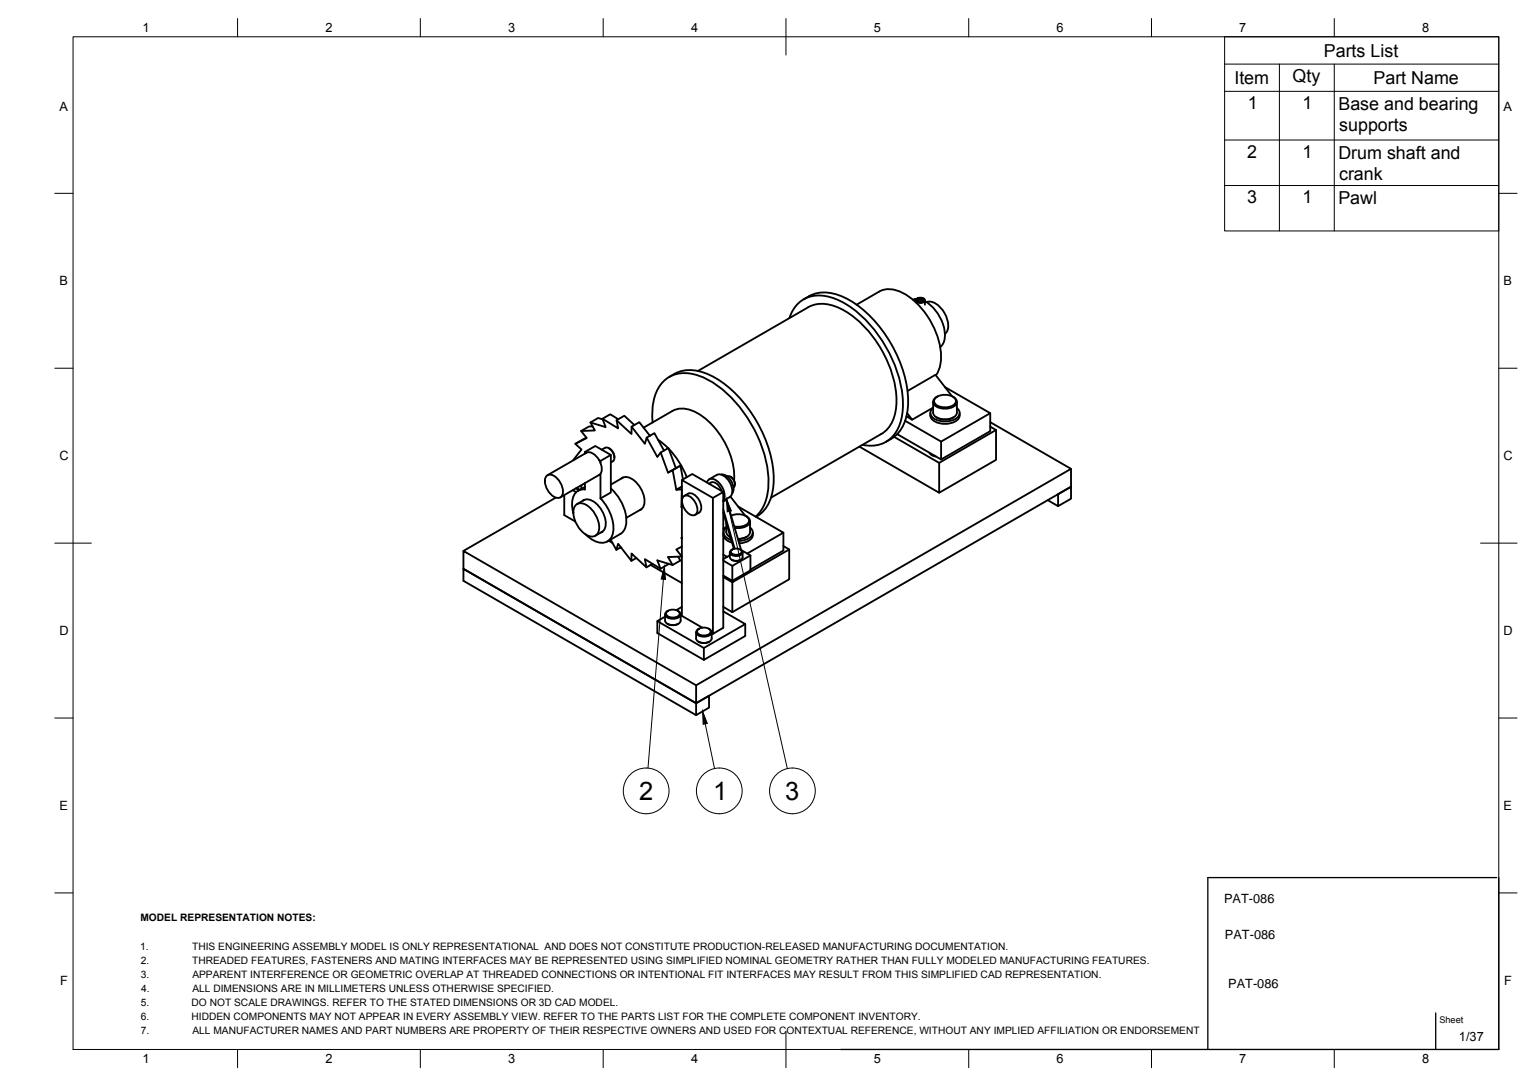
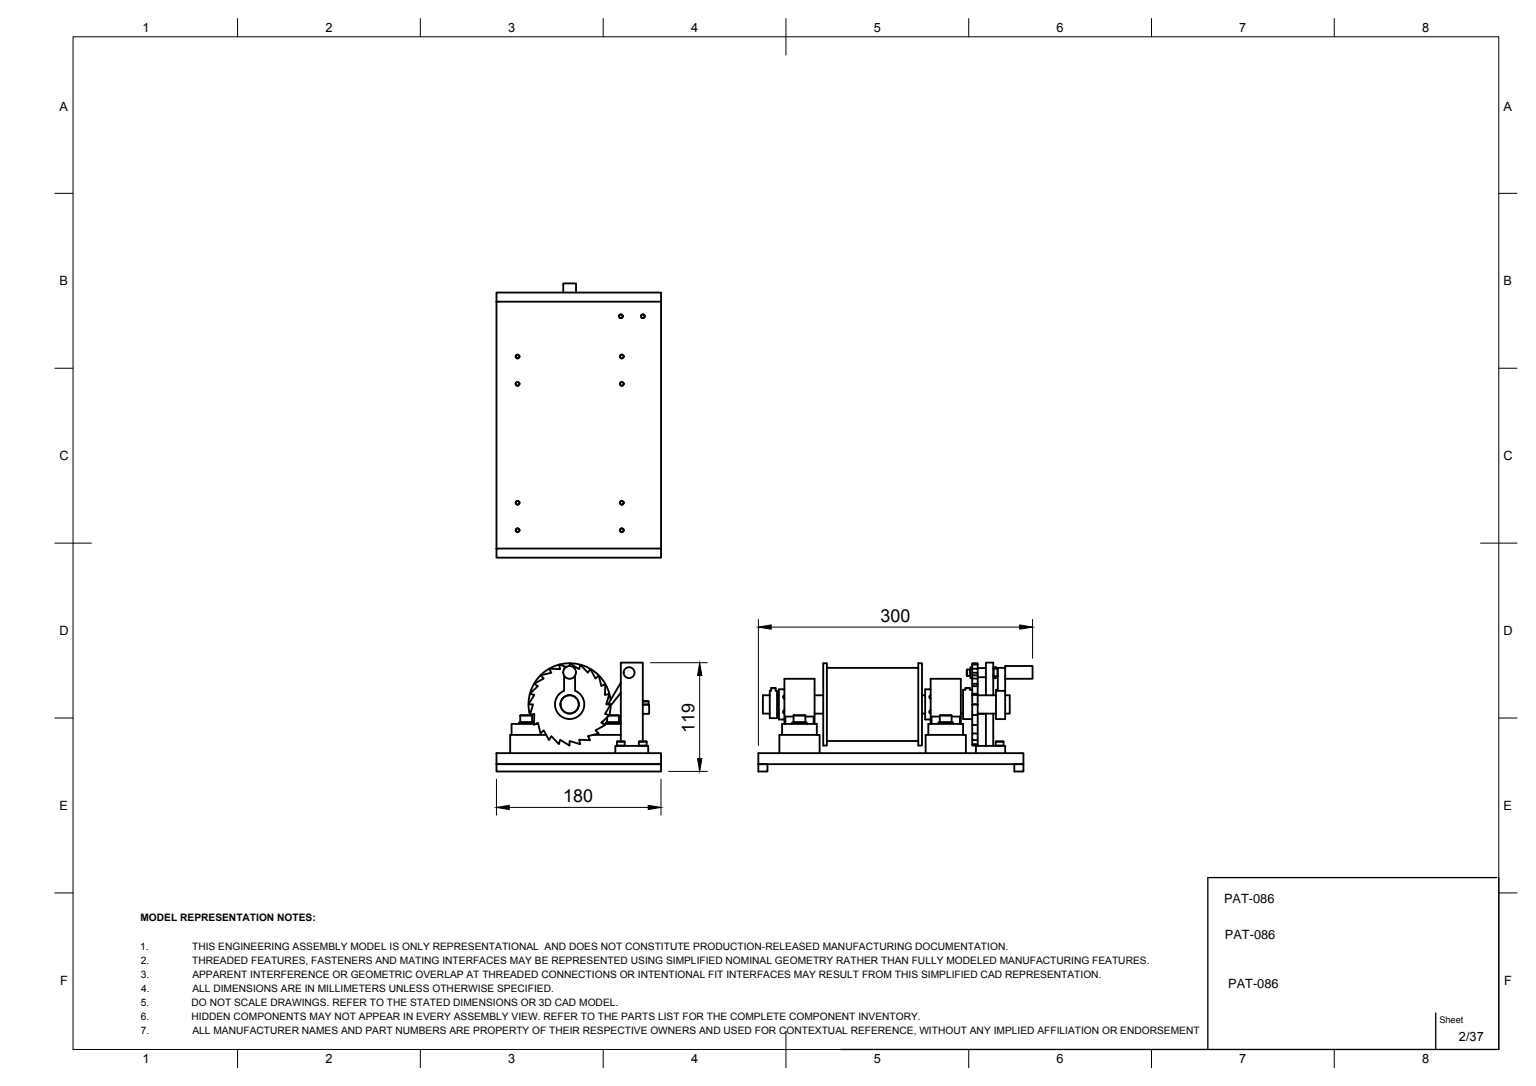
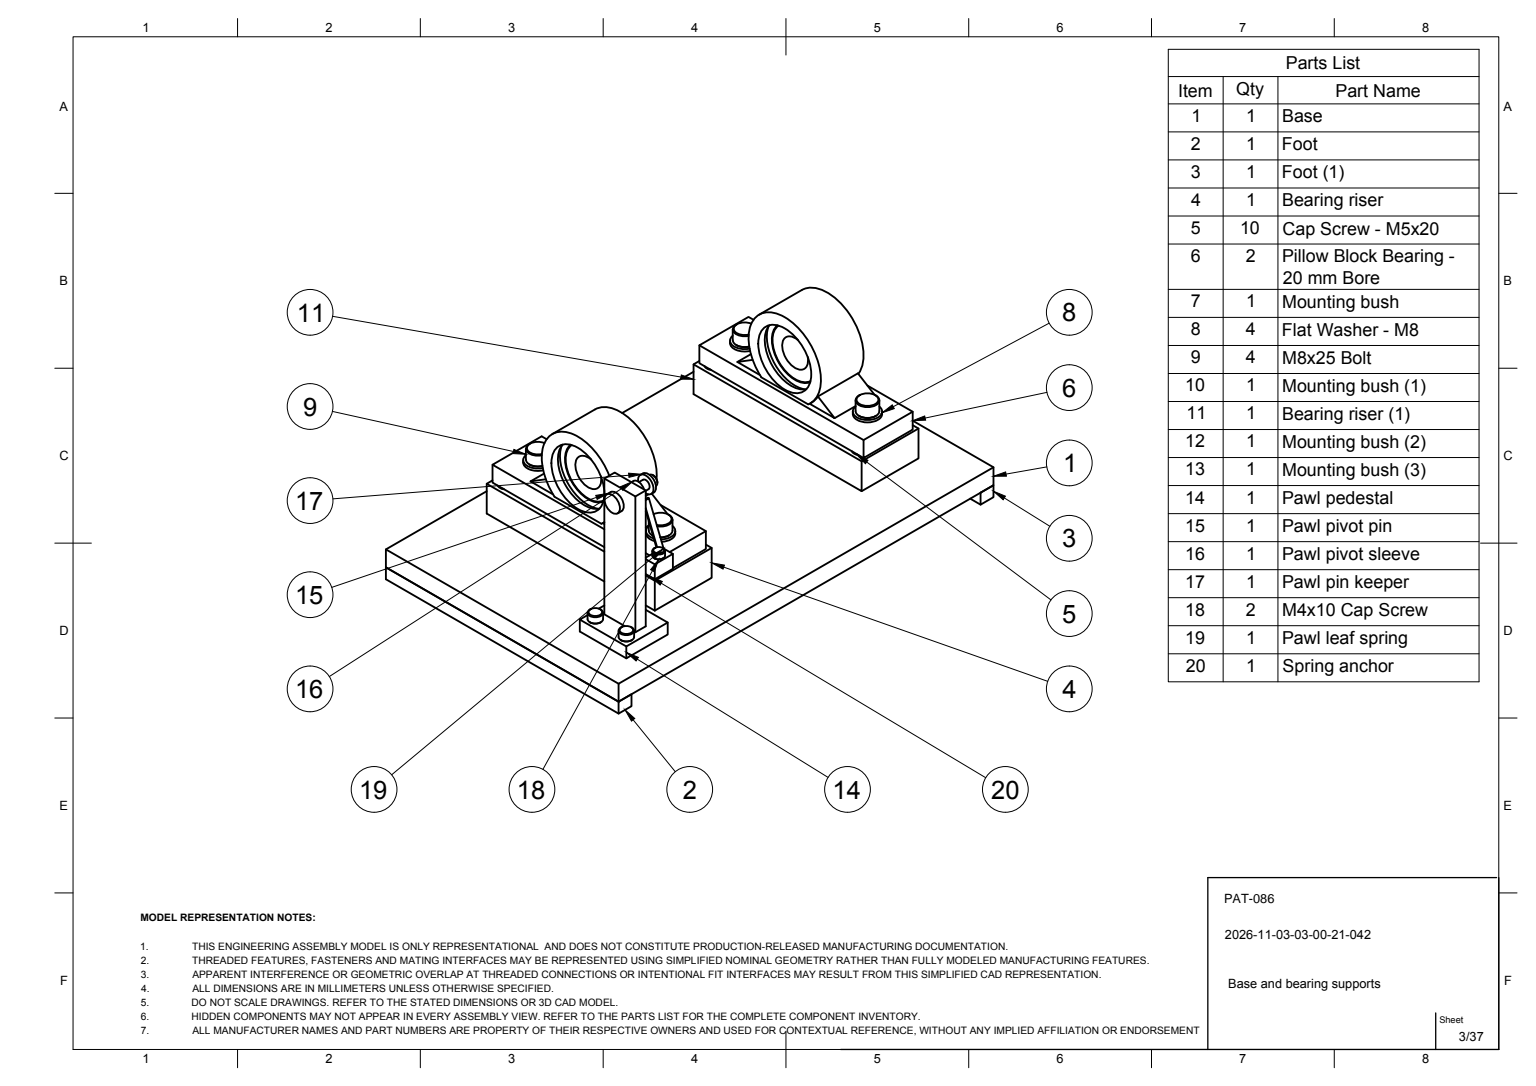
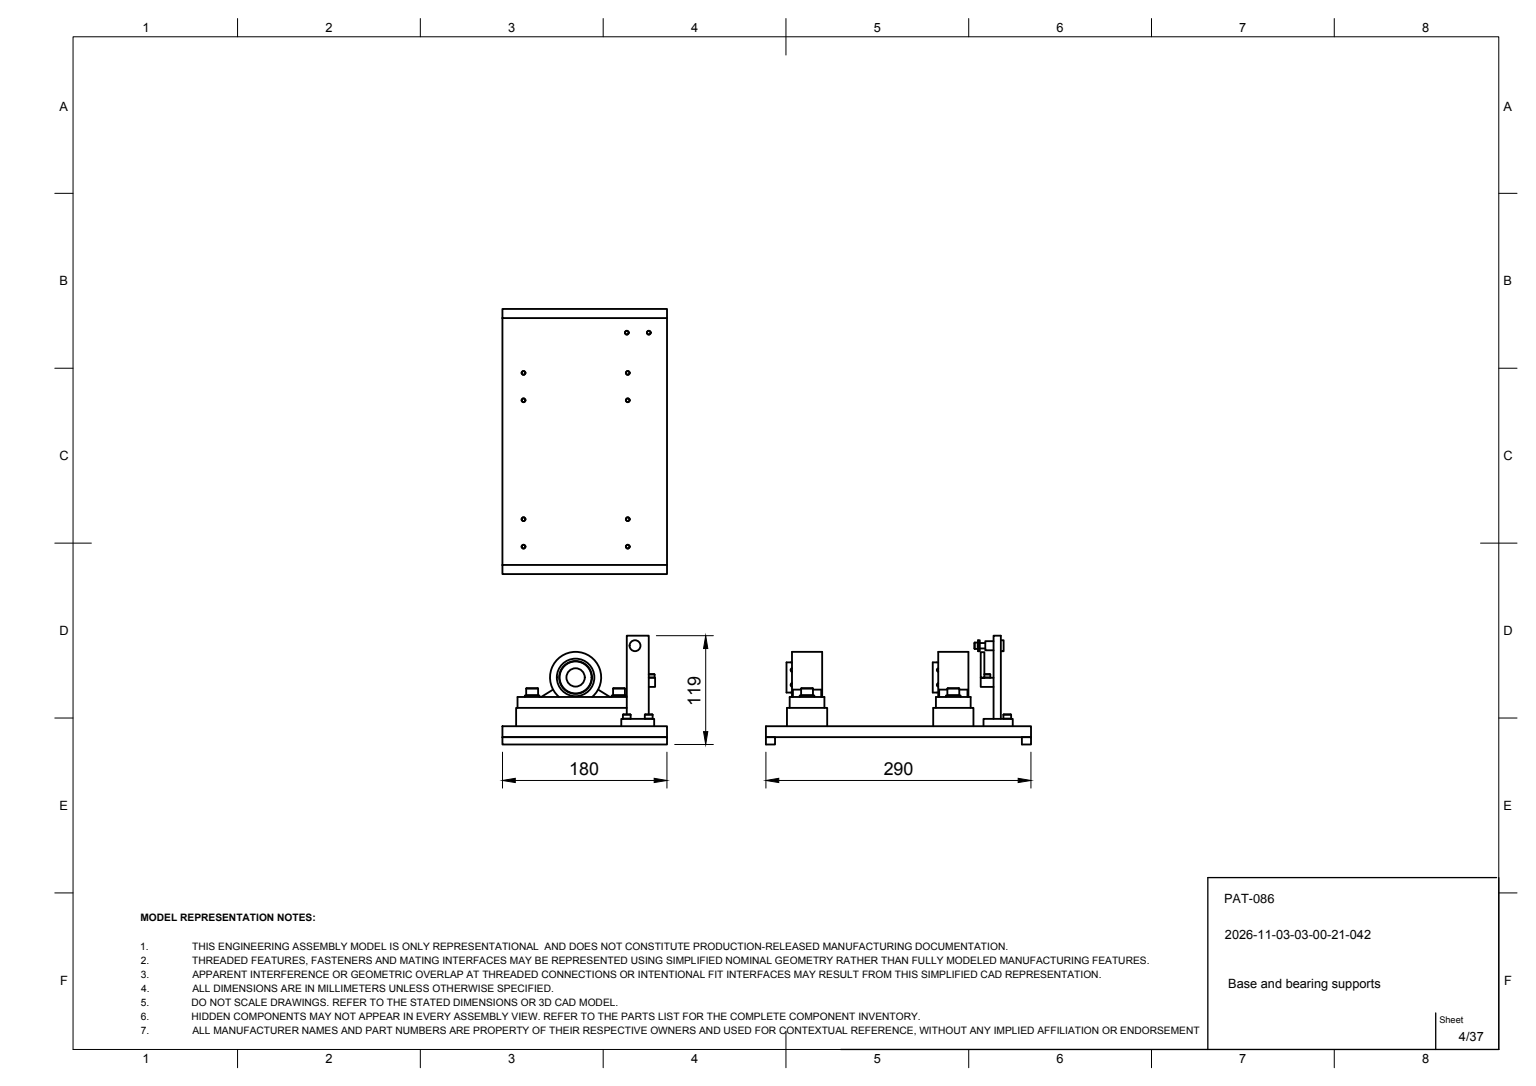
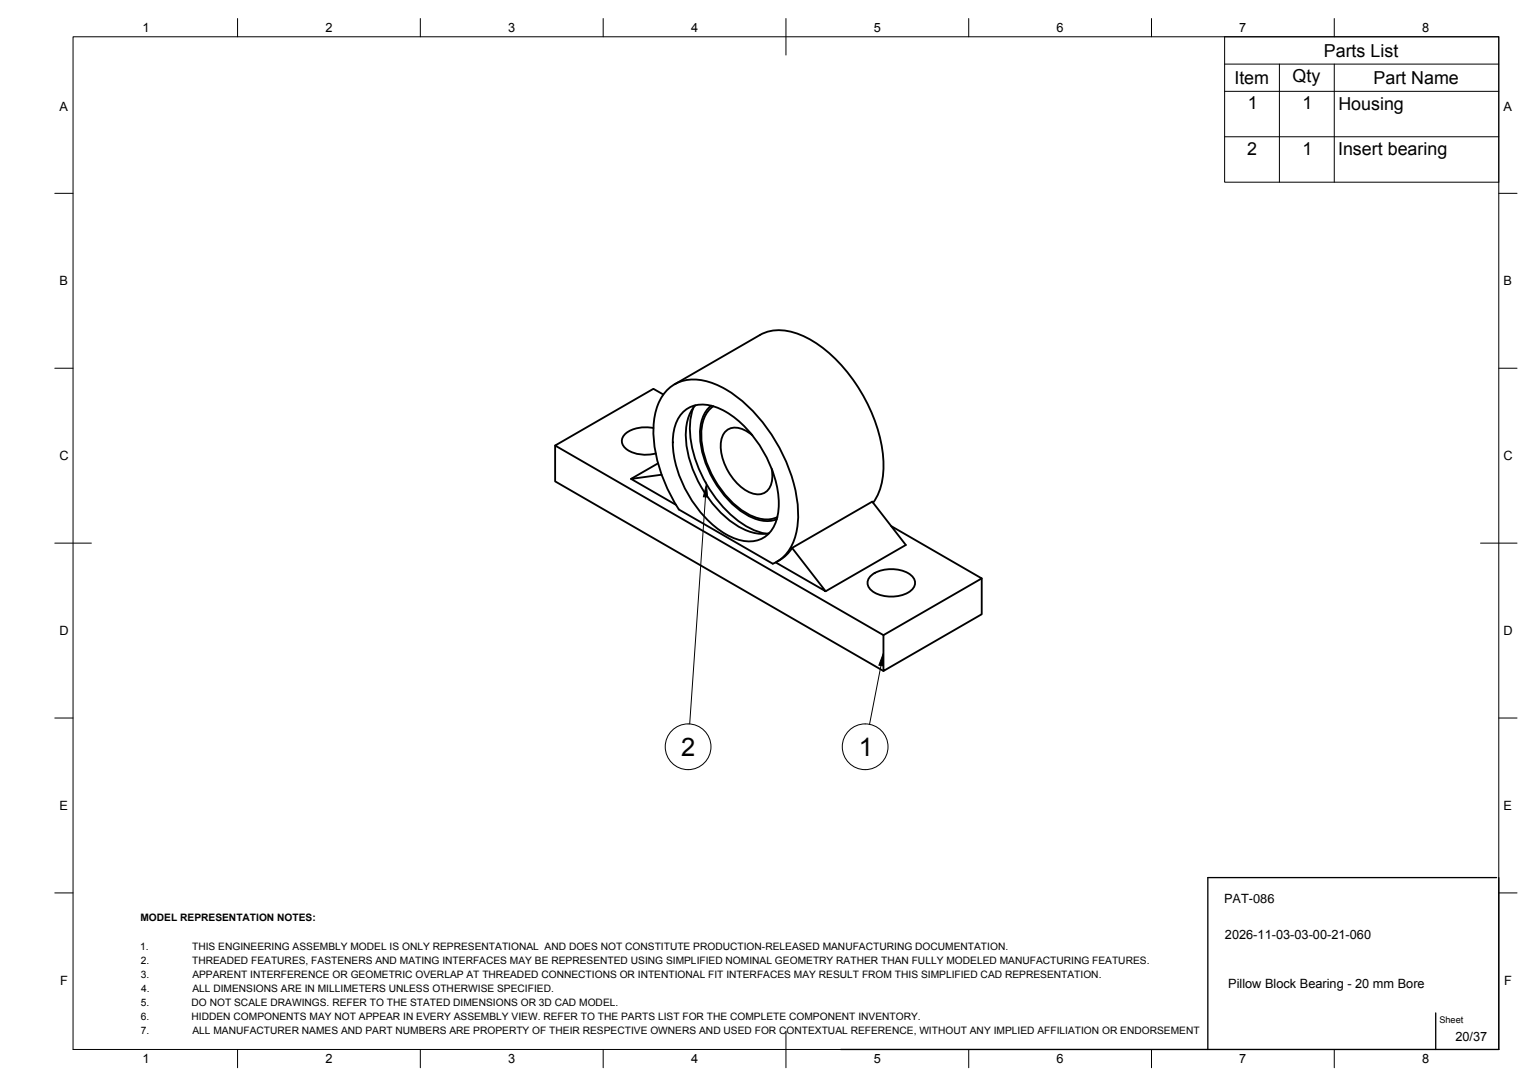
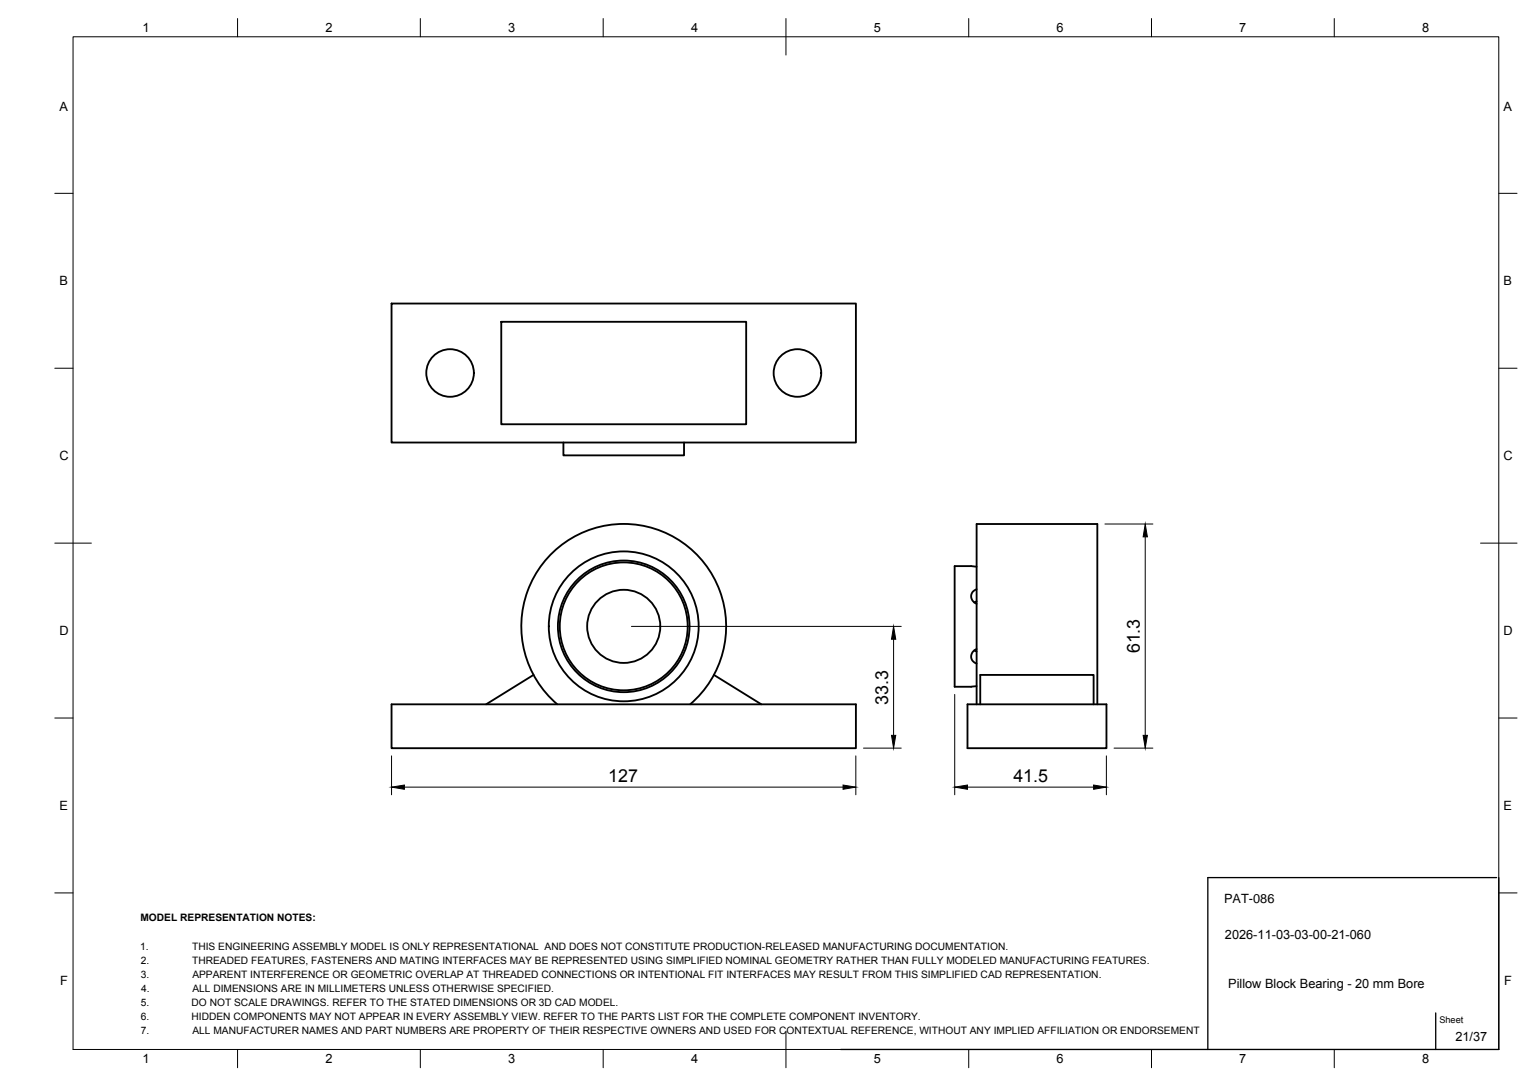
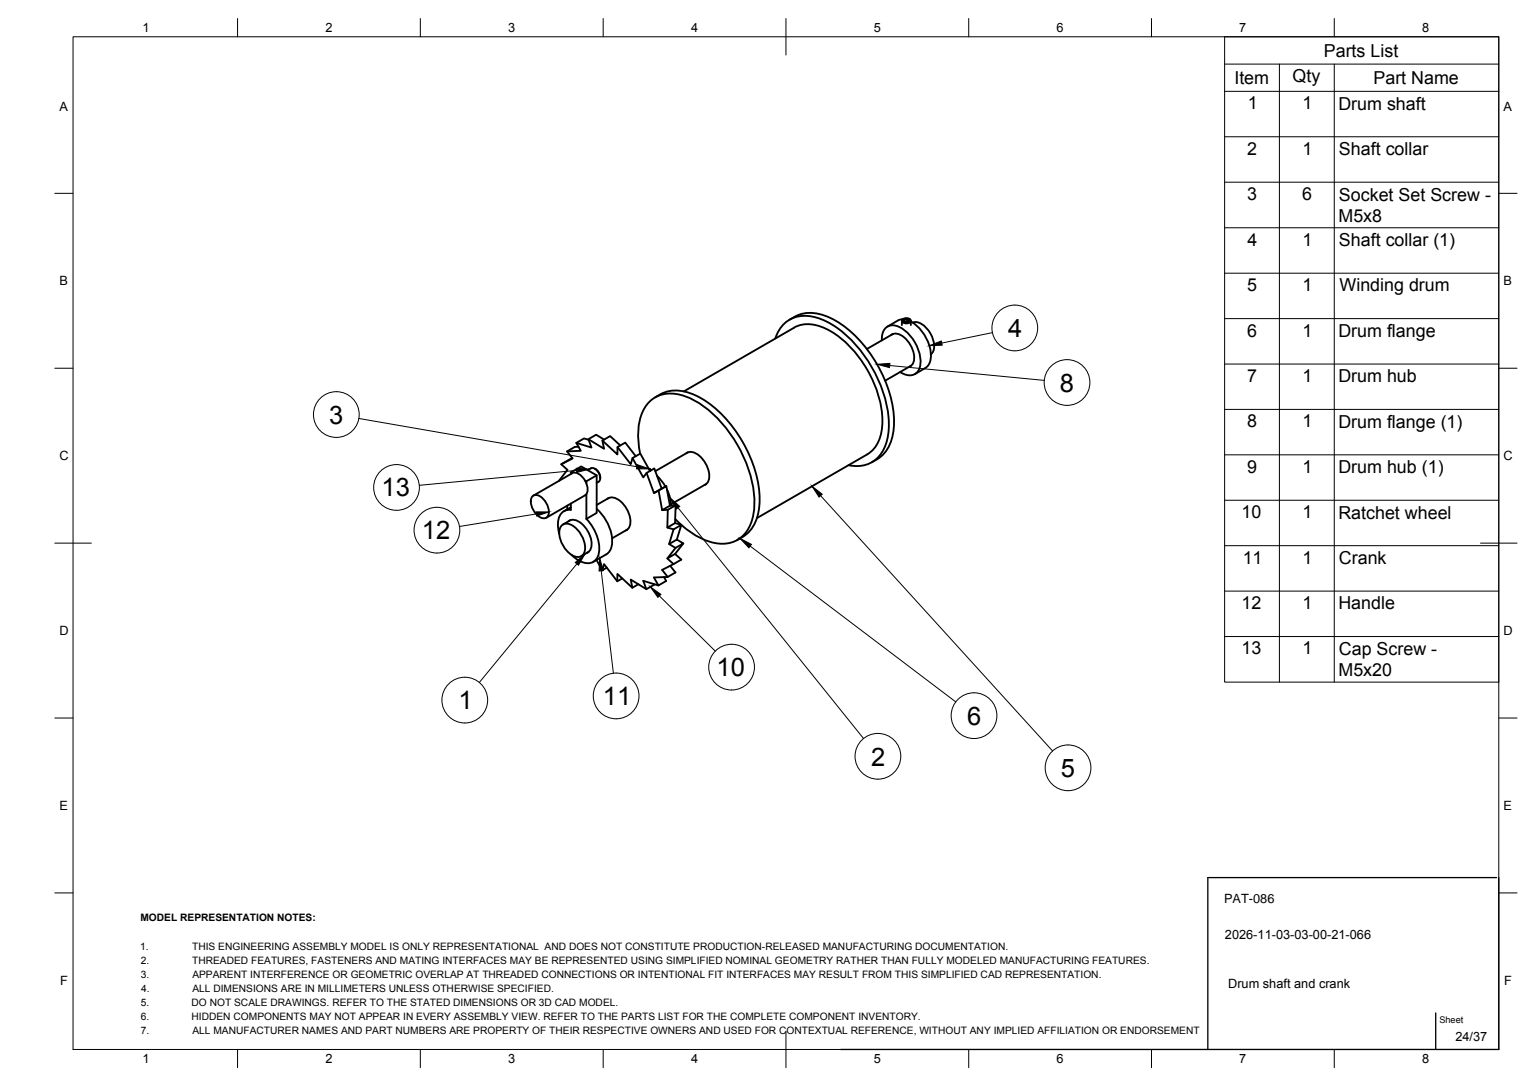
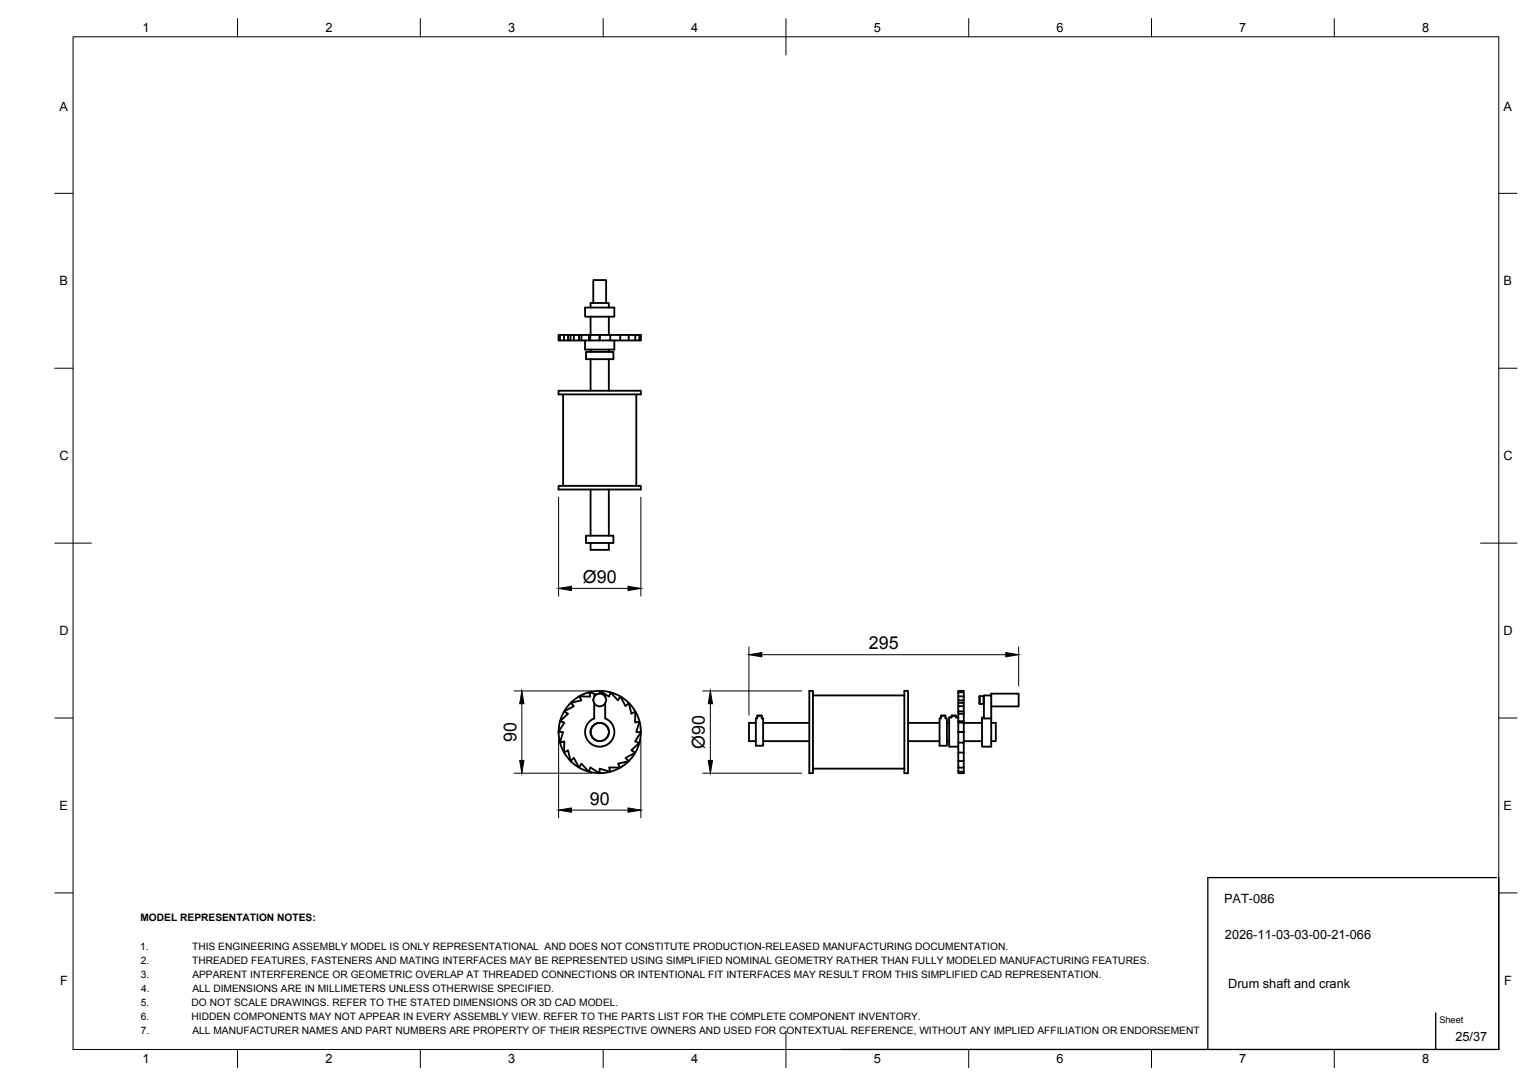
ISO-10303-21;
HEADER;
/* Generated by software containing ST-Developer
 * from STEP Tools, Inc. (www.steptools.com) 
 */

FILE_DESCRIPTION(
/* description */ ('Ratchet and pawl hand winch drum'),
/* implementation_level */ '2;1');

FILE_NAME(
/* name */ 'PAT-086',
/* time_stamp */ '2026-10-27T12:42:58-07:00',
/* author */ (''),
/* organization */ (''),
/* preprocessor_version */ 'ST-DEVELOPER v20.2',
/* originating_system */ 'Autodesk Translation Framework v15.17.0.0',
/* authorisation */ '');

FILE_SCHEMA (('AUTOMOTIVE_DESIGN { 1 0 10303 214 3 1 1 }'));
ENDSEC;

DATA;
#10=MECHANICAL_DESIGN_GEOMETRIC_PRESENTATION_REPRESENTATION('',(#389,#390,
#391,#392,#393,#394,#395,#396,#397,#398,#399,#400,#401,#402,#403,#404,#405,
#406,#407,#408,#409,#410,#411,#412,#413,#414,#415,#416,#417,#418,#419,#420,
#421,#422,#423),#11801);
#11=CONICAL_SURFACE('',#7014,0.625,0.785398163397448);
#12=CONICAL_SURFACE('',#7018,0.635,0.785398163397449);
#13=CONICAL_SURFACE('',#7022,0.41,0.463647609000806);
#14=CONICAL_SURFACE('',#7038,0.325,0.785398163397448);
#15=CONICAL_SURFACE('',#7042,0.335,0.785398163397448);
#16=CONICAL_SURFACE('',#7046,0.21,0.463647609000806);
#17=CONICAL_SURFACE('',#7253,0.235,0.785398163397448);
#18=CONICAL_SURFACE('',#7257,0.2125,0.785398163397448);
#19=CONICAL_SURFACE('',#7263,0.4,0.785398163397448);
#20=CONICAL_SURFACE('',#7267,0.41,0.785398163397448);
#21=CONICAL_SURFACE('',#7271,0.26,0.463647609000806);
#22=CONICAL_SURFACE('',#7275,0.225,0.785398163397448);
#23=ORIENTED_CLOSED_SHELL('',*,#6285,.F.);
#24=ORIENTED_CLOSED_SHELL('',*,#6287,.F.);
#25=ORIENTED_CLOSED_SHELL('',*,#6302,.F.);
#26=BREP_WITH_VOIDS('Body1',#6286,(#23));
#27=BREP_WITH_VOIDS('Body1',#6288,(#24));
#28=BREP_WITH_VOIDS('Body1',#6301,(#25));
#29=ITEM_DEFINED_TRANSFORMATION($,$,#6921,#6990);
#30=ITEM_DEFINED_TRANSFORMATION($,$,#6962,#6991);
#31=ITEM_DEFINED_TRANSFORMATION($,$,#6681,#7286);
#32=ITEM_DEFINED_TRANSFORMATION($,$,#6718,#7287);
#33=ITEM_DEFINED_TRANSFORMATION($,$,#6725,#7288);
#34=ITEM_DEFINED_TRANSFORMATION($,$,#6732,#7289);
#35=ITEM_DEFINED_TRANSFORMATION($,$,#6773,#7290);
#36=ITEM_DEFINED_TRANSFORMATION($,$,#6782,#7291);
#37=ITEM_DEFINED_TRANSFORMATION($,$,#6791,#7292);
#38=ITEM_DEFINED_TRANSFORMATION($,$,#6832,#7293);
#39=ITEM_DEFINED_TRANSFORMATION($,$,#6841,#7294);
#40=ITEM_DEFINED_TRANSFORMATION($,$,#6850,#7295);
#41=ITEM_DEFINED_TRANSFORMATION($,$,#6871,#7296);
#42=ITEM_DEFINED_TRANSFORMATION($,$,#6885,#7297);
#43=ITEM_DEFINED_TRANSFORMATION($,$,#6894,#7298);
#44=ITEM_DEFINED_TRANSFORMATION($,$,#6903,#7299);
#45=ITEM_DEFINED_TRANSFORMATION($,$,#6910,#7300);
#46=ITEM_DEFINED_TRANSFORMATION($,$,#7260,#7301);
#47=ITEM_DEFINED_TRANSFORMATION($,$,#7260,#7302);
#48=ITEM_DEFINED_TRANSFORMATION($,$,#7260,#7303);
#49=ITEM_DEFINED_TRANSFORMATION($,$,#7260,#7304);
#50=ITEM_DEFINED_TRANSFORMATION($,$,#6920,#7305);
#51=ITEM_DEFINED_TRANSFORMATION($,$,#6992,#7306);
#52=ITEM_DEFINED_TRANSFORMATION($,$,#7001,#7307);
#53=ITEM_DEFINED_TRANSFORMATION($,$,#6992,#7308);
#54=ITEM_DEFINED_TRANSFORMATION($,$,#7001,#7309);
#55=ITEM_DEFINED_TRANSFORMATION($,$,#7260,#7310);
#56=ITEM_DEFINED_TRANSFORMATION($,$,#7260,#7311);
#57=ITEM_DEFINED_TRANSFORMATION($,$,#7260,#7312);
#58=ITEM_DEFINED_TRANSFORMATION($,$,#7260,#7313);
#59=ITEM_DEFINED_TRANSFORMATION($,$,#6920,#7314);
#60=ITEM_DEFINED_TRANSFORMATION($,$,#6992,#7315);
#61=ITEM_DEFINED_TRANSFORMATION($,$,#7001,#7316);
#62=ITEM_DEFINED_TRANSFORMATION($,$,#6992,#7317);
#63=ITEM_DEFINED_TRANSFORMATION($,$,#7001,#7318);
#64=ITEM_DEFINED_TRANSFORMATION($,$,#7260,#7319);
#65=ITEM_DEFINED_TRANSFORMATION($,$,#7260,#7320);
#66=ITEM_DEFINED_TRANSFORMATION($,$,#7025,#7321);
#67=ITEM_DEFINED_TRANSFORMATION($,$,#7025,#7322);
#68=ITEM_DEFINED_TRANSFORMATION($,$,#7050,#7323);
#69=ITEM_DEFINED_TRANSFORMATION($,$,#7056,#7324);
#70=ITEM_DEFINED_TRANSFORMATION($,$,#7071,#7325);
#71=ITEM_DEFINED_TRANSFORMATION($,$,#7086,#7326);
#72=ITEM_DEFINED_TRANSFORMATION($,$,#7095,#7327);
#73=ITEM_DEFINED_TRANSFORMATION($,$,#7104,#7328);
#74=ITEM_DEFINED_TRANSFORMATION($,$,#7119,#7329);
#75=ITEM_DEFINED_TRANSFORMATION($,$,#7128,#7330);
#76=ITEM_DEFINED_TRANSFORMATION($,$,#7143,#7331);
#77=ITEM_DEFINED_TRANSFORMATION($,$,#7207,#7332);
#78=ITEM_DEFINED_TRANSFORMATION($,$,#7233,#7333);
#79=ITEM_DEFINED_TRANSFORMATION($,$,#7243,#7334);
#80=ITEM_DEFINED_TRANSFORMATION($,$,#7243,#7335);
#81=ITEM_DEFINED_TRANSFORMATION($,$,#7243,#7336);
#82=ITEM_DEFINED_TRANSFORMATION($,$,#7243,#7337);
#83=ITEM_DEFINED_TRANSFORMATION($,$,#7243,#7338);
#84=ITEM_DEFINED_TRANSFORMATION($,$,#7243,#7339);
#85=ITEM_DEFINED_TRANSFORMATION($,$,#7260,#7340);
#86=ITEM_DEFINED_TRANSFORMATION($,$,#7342,#7354);
#87=ITEM_DEFINED_TRANSFORMATION($,$,#6680,#7355);
#88=ITEM_DEFINED_TRANSFORMATION($,$,#7049,#7356);
#89=ITEM_DEFINED_TRANSFORMATION($,$,#7341,#7357);
#90=(
REPRESENTATION_RELATIONSHIP($,$,#11963,#11962)
REPRESENTATION_RELATIONSHIP_WITH_TRANSFORMATION(#29)
SHAPE_REPRESENTATION_RELATIONSHIP()
);
#91=(
REPRESENTATION_RELATIONSHIP($,$,#11964,#11962)
REPRESENTATION_RELATIONSHIP_WITH_TRANSFORMATION(#30)
SHAPE_REPRESENTATION_RELATIONSHIP()
);
#92=(
REPRESENTATION_RELATIONSHIP($,$,#11947,#11946)
REPRESENTATION_RELATIONSHIP_WITH_TRANSFORMATION(#31)
SHAPE_REPRESENTATION_RELATIONSHIP()
);
#93=(
REPRESENTATION_RELATIONSHIP($,$,#11948,#11946)
REPRESENTATION_RELATIONSHIP_WITH_TRANSFORMATION(#32)
SHAPE_REPRESENTATION_RELATIONSHIP()
);
#94=(
REPRESENTATION_RELATIONSHIP($,$,#11949,#11946)
REPRESENTATION_RELATIONSHIP_WITH_TRANSFORMATION(#33)
SHAPE_REPRESENTATION_RELATIONSHIP()
);
#95=(
REPRESENTATION_RELATIONSHIP($,$,#11950,#11946)
REPRESENTATION_RELATIONSHIP_WITH_TRANSFORMATION(#34)
SHAPE_REPRESENTATION_RELATIONSHIP()
);
#96=(
REPRESENTATION_RELATIONSHIP($,$,#11951,#11946)
REPRESENTATION_RELATIONSHIP_WITH_TRANSFORMATION(#35)
SHAPE_REPRESENTATION_RELATIONSHIP()
);
#97=(
REPRESENTATION_RELATIONSHIP($,$,#11952,#11946)
REPRESENTATION_RELATIONSHIP_WITH_TRANSFORMATION(#36)
SHAPE_REPRESENTATION_RELATIONSHIP()
);
#98=(
REPRESENTATION_RELATIONSHIP($,$,#11953,#11946)
REPRESENTATION_RELATIONSHIP_WITH_TRANSFORMATION(#37)
SHAPE_REPRESENTATION_RELATIONSHIP()
);
#99=(
REPRESENTATION_RELATIONSHIP($,$,#11954,#11946)
REPRESENTATION_RELATIONSHIP_WITH_TRANSFORMATION(#38)
SHAPE_REPRESENTATION_RELATIONSHIP()
);
#100=(
REPRESENTATION_RELATIONSHIP($,$,#11955,#11946)
REPRESENTATION_RELATIONSHIP_WITH_TRANSFORMATION(#39)
SHAPE_REPRESENTATION_RELATIONSHIP()
);
#101=(
REPRESENTATION_RELATIONSHIP($,$,#11956,#11946)
REPRESENTATION_RELATIONSHIP_WITH_TRANSFORMATION(#40)
SHAPE_REPRESENTATION_RELATIONSHIP()
);
#102=(
REPRESENTATION_RELATIONSHIP($,$,#11957,#11946)
REPRESENTATION_RELATIONSHIP_WITH_TRANSFORMATION(#41)
SHAPE_REPRESENTATION_RELATIONSHIP()
);
#103=(
REPRESENTATION_RELATIONSHIP($,$,#11958,#11946)
REPRESENTATION_RELATIONSHIP_WITH_TRANSFORMATION(#42)
SHAPE_REPRESENTATION_RELATIONSHIP()
);
#104=(
REPRESENTATION_RELATIONSHIP($,$,#11959,#11946)
REPRESENTATION_RELATIONSHIP_WITH_TRANSFORMATION(#43)
SHAPE_REPRESENTATION_RELATIONSHIP()
);
#105=(
REPRESENTATION_RELATIONSHIP($,$,#11960,#11946)
REPRESENTATION_RELATIONSHIP_WITH_TRANSFORMATION(#44)
SHAPE_REPRESENTATION_RELATIONSHIP()
);
#106=(
REPRESENTATION_RELATIONSHIP($,$,#11961,#11946)
REPRESENTATION_RELATIONSHIP_WITH_TRANSFORMATION(#45)
SHAPE_REPRESENTATION_RELATIONSHIP()
);
#107=(
REPRESENTATION_RELATIONSHIP($,$,#11981,#11946)
REPRESENTATION_RELATIONSHIP_WITH_TRANSFORMATION(#46)
SHAPE_REPRESENTATION_RELATIONSHIP()
);
#108=(
REPRESENTATION_RELATIONSHIP($,$,#11981,#11946)
REPRESENTATION_RELATIONSHIP_WITH_TRANSFORMATION(#47)
SHAPE_REPRESENTATION_RELATIONSHIP()
);
#109=(
REPRESENTATION_RELATIONSHIP($,$,#11981,#11946)
REPRESENTATION_RELATIONSHIP_WITH_TRANSFORMATION(#48)
SHAPE_REPRESENTATION_RELATIONSHIP()
);
#110=(
REPRESENTATION_RELATIONSHIP($,$,#11981,#11946)
REPRESENTATION_RELATIONSHIP_WITH_TRANSFORMATION(#49)
SHAPE_REPRESENTATION_RELATIONSHIP()
);
#111=(
REPRESENTATION_RELATIONSHIP($,$,#11962,#11946)
REPRESENTATION_RELATIONSHIP_WITH_TRANSFORMATION(#50)
SHAPE_REPRESENTATION_RELATIONSHIP()
);
#112=(
REPRESENTATION_RELATIONSHIP($,$,#11965,#11946)
REPRESENTATION_RELATIONSHIP_WITH_TRANSFORMATION(#51)
SHAPE_REPRESENTATION_RELATIONSHIP()
);
#113=(
REPRESENTATION_RELATIONSHIP($,$,#11966,#11946)
REPRESENTATION_RELATIONSHIP_WITH_TRANSFORMATION(#52)
SHAPE_REPRESENTATION_RELATIONSHIP()
);
#114=(
REPRESENTATION_RELATIONSHIP($,$,#11965,#11946)
REPRESENTATION_RELATIONSHIP_WITH_TRANSFORMATION(#53)
SHAPE_REPRESENTATION_RELATIONSHIP()
);
#115=(
REPRESENTATION_RELATIONSHIP($,$,#11966,#11946)
REPRESENTATION_RELATIONSHIP_WITH_TRANSFORMATION(#54)
SHAPE_REPRESENTATION_RELATIONSHIP()
);
#116=(
REPRESENTATION_RELATIONSHIP($,$,#11981,#11946)
REPRESENTATION_RELATIONSHIP_WITH_TRANSFORMATION(#55)
SHAPE_REPRESENTATION_RELATIONSHIP()
);
#117=(
REPRESENTATION_RELATIONSHIP($,$,#11981,#11946)
REPRESENTATION_RELATIONSHIP_WITH_TRANSFORMATION(#56)
SHAPE_REPRESENTATION_RELATIONSHIP()
);
#118=(
REPRESENTATION_RELATIONSHIP($,$,#11981,#11946)
REPRESENTATION_RELATIONSHIP_WITH_TRANSFORMATION(#57)
SHAPE_REPRESENTATION_RELATIONSHIP()
);
#119=(
REPRESENTATION_RELATIONSHIP($,$,#11981,#11946)
REPRESENTATION_RELATIONSHIP_WITH_TRANSFORMATION(#58)
SHAPE_REPRESENTATION_RELATIONSHIP()
);
#120=(
REPRESENTATION_RELATIONSHIP($,$,#11962,#11946)
REPRESENTATION_RELATIONSHIP_WITH_TRANSFORMATION(#59)
SHAPE_REPRESENTATION_RELATIONSHIP()
);
#121=(
REPRESENTATION_RELATIONSHIP($,$,#11965,#11946)
REPRESENTATION_RELATIONSHIP_WITH_TRANSFORMATION(#60)
SHAPE_REPRESENTATION_RELATIONSHIP()
);
#122=(
REPRESENTATION_RELATIONSHIP($,$,#11966,#11946)
REPRESENTATION_RELATIONSHIP_WITH_TRANSFORMATION(#61)
SHAPE_REPRESENTATION_RELATIONSHIP()
);
#123=(
REPRESENTATION_RELATIONSHIP($,$,#11965,#11946)
REPRESENTATION_RELATIONSHIP_WITH_TRANSFORMATION(#62)
SHAPE_REPRESENTATION_RELATIONSHIP()
);
#124=(
REPRESENTATION_RELATIONSHIP($,$,#11966,#11946)
REPRESENTATION_RELATIONSHIP_WITH_TRANSFORMATION(#63)
SHAPE_REPRESENTATION_RELATIONSHIP()
);
#125=(
REPRESENTATION_RELATIONSHIP($,$,#11981,#11946)
REPRESENTATION_RELATIONSHIP_WITH_TRANSFORMATION(#64)
SHAPE_REPRESENTATION_RELATIONSHIP()
);
#126=(
REPRESENTATION_RELATIONSHIP($,$,#11981,#11946)
REPRESENTATION_RELATIONSHIP_WITH_TRANSFORMATION(#65)
SHAPE_REPRESENTATION_RELATIONSHIP()
);
#127=(
REPRESENTATION_RELATIONSHIP($,$,#11967,#11946)
REPRESENTATION_RELATIONSHIP_WITH_TRANSFORMATION(#66)
SHAPE_REPRESENTATION_RELATIONSHIP()
);
#128=(
REPRESENTATION_RELATIONSHIP($,$,#11967,#11946)
REPRESENTATION_RELATIONSHIP_WITH_TRANSFORMATION(#67)
SHAPE_REPRESENTATION_RELATIONSHIP()
);
#129=(
REPRESENTATION_RELATIONSHIP($,$,#11969,#11968)
REPRESENTATION_RELATIONSHIP_WITH_TRANSFORMATION(#68)
SHAPE_REPRESENTATION_RELATIONSHIP()
);
#130=(
REPRESENTATION_RELATIONSHIP($,$,#11970,#11968)
REPRESENTATION_RELATIONSHIP_WITH_TRANSFORMATION(#69)
SHAPE_REPRESENTATION_RELATIONSHIP()
);
#131=(
REPRESENTATION_RELATIONSHIP($,$,#11971,#11968)
REPRESENTATION_RELATIONSHIP_WITH_TRANSFORMATION(#70)
SHAPE_REPRESENTATION_RELATIONSHIP()
);
#132=(
REPRESENTATION_RELATIONSHIP($,$,#11972,#11968)
REPRESENTATION_RELATIONSHIP_WITH_TRANSFORMATION(#71)
SHAPE_REPRESENTATION_RELATIONSHIP()
);
#133=(
REPRESENTATION_RELATIONSHIP($,$,#11973,#11968)
REPRESENTATION_RELATIONSHIP_WITH_TRANSFORMATION(#72)
SHAPE_REPRESENTATION_RELATIONSHIP()
);
#134=(
REPRESENTATION_RELATIONSHIP($,$,#11974,#11968)
REPRESENTATION_RELATIONSHIP_WITH_TRANSFORMATION(#73)
SHAPE_REPRESENTATION_RELATIONSHIP()
);
#135=(
REPRESENTATION_RELATIONSHIP($,$,#11975,#11968)
REPRESENTATION_RELATIONSHIP_WITH_TRANSFORMATION(#74)
SHAPE_REPRESENTATION_RELATIONSHIP()
);
#136=(
REPRESENTATION_RELATIONSHIP($,$,#11976,#11968)
REPRESENTATION_RELATIONSHIP_WITH_TRANSFORMATION(#75)
SHAPE_REPRESENTATION_RELATIONSHIP()
);
#137=(
REPRESENTATION_RELATIONSHIP($,$,#11977,#11968)
REPRESENTATION_RELATIONSHIP_WITH_TRANSFORMATION(#76)
SHAPE_REPRESENTATION_RELATIONSHIP()
);
#138=(
REPRESENTATION_RELATIONSHIP($,$,#11978,#11968)
REPRESENTATION_RELATIONSHIP_WITH_TRANSFORMATION(#77)
SHAPE_REPRESENTATION_RELATIONSHIP()
);
#139=(
REPRESENTATION_RELATIONSHIP($,$,#11979,#11968)
REPRESENTATION_RELATIONSHIP_WITH_TRANSFORMATION(#78)
SHAPE_REPRESENTATION_RELATIONSHIP()
);
#140=(
REPRESENTATION_RELATIONSHIP($,$,#11980,#11968)
REPRESENTATION_RELATIONSHIP_WITH_TRANSFORMATION(#79)
SHAPE_REPRESENTATION_RELATIONSHIP()
);
#141=(
REPRESENTATION_RELATIONSHIP($,$,#11980,#11968)
REPRESENTATION_RELATIONSHIP_WITH_TRANSFORMATION(#80)
SHAPE_REPRESENTATION_RELATIONSHIP()
);
#142=(
REPRESENTATION_RELATIONSHIP($,$,#11980,#11968)
REPRESENTATION_RELATIONSHIP_WITH_TRANSFORMATION(#81)
SHAPE_REPRESENTATION_RELATIONSHIP()
);
#143=(
REPRESENTATION_RELATIONSHIP($,$,#11980,#11968)
REPRESENTATION_RELATIONSHIP_WITH_TRANSFORMATION(#82)
SHAPE_REPRESENTATION_RELATIONSHIP()
);
#144=(
REPRESENTATION_RELATIONSHIP($,$,#11980,#11968)
REPRESENTATION_RELATIONSHIP_WITH_TRANSFORMATION(#83)
SHAPE_REPRESENTATION_RELATIONSHIP()
);
#145=(
REPRESENTATION_RELATIONSHIP($,$,#11980,#11968)
REPRESENTATION_RELATIONSHIP_WITH_TRANSFORMATION(#84)
SHAPE_REPRESENTATION_RELATIONSHIP()
);
#146=(
REPRESENTATION_RELATIONSHIP($,$,#11981,#11968)
REPRESENTATION_RELATIONSHIP_WITH_TRANSFORMATION(#85)
SHAPE_REPRESENTATION_RELATIONSHIP()
);
#147=(
REPRESENTATION_RELATIONSHIP($,$,#11983,#11982)
REPRESENTATION_RELATIONSHIP_WITH_TRANSFORMATION(#86)
SHAPE_REPRESENTATION_RELATIONSHIP()
);
#148=(
REPRESENTATION_RELATIONSHIP($,$,#11946,#11945)
REPRESENTATION_RELATIONSHIP_WITH_TRANSFORMATION(#87)
SHAPE_REPRESENTATION_RELATIONSHIP()
);
#149=(
REPRESENTATION_RELATIONSHIP($,$,#11968,#11945)
REPRESENTATION_RELATIONSHIP_WITH_TRANSFORMATION(#88)
SHAPE_REPRESENTATION_RELATIONSHIP()
);
#150=(
REPRESENTATION_RELATIONSHIP($,$,#11982,#11945)
REPRESENTATION_RELATIONSHIP_WITH_TRANSFORMATION(#89)
SHAPE_REPRESENTATION_RELATIONSHIP()
);
#151=CONTEXT_DEPENDENT_SHAPE_REPRESENTATION(#90,#11865);
#152=CONTEXT_DEPENDENT_SHAPE_REPRESENTATION(#91,#11866);
#153=CONTEXT_DEPENDENT_SHAPE_REPRESENTATION(#92,#11884);
#154=CONTEXT_DEPENDENT_SHAPE_REPRESENTATION(#93,#11885);
#155=CONTEXT_DEPENDENT_SHAPE_REPRESENTATION(#94,#11886);
#156=CONTEXT_DEPENDENT_SHAPE_REPRESENTATION(#95,#11887);
#157=CONTEXT_DEPENDENT_SHAPE_REPRESENTATION(#96,#11888);
#158=CONTEXT_DEPENDENT_SHAPE_REPRESENTATION(#97,#11889);
#159=CONTEXT_DEPENDENT_SHAPE_REPRESENTATION(#98,#11890);
#160=CONTEXT_DEPENDENT_SHAPE_REPRESENTATION(#99,#11891);
#161=CONTEXT_DEPENDENT_SHAPE_REPRESENTATION(#100,#11892);
#162=CONTEXT_DEPENDENT_SHAPE_REPRESENTATION(#101,#11893);
#163=CONTEXT_DEPENDENT_SHAPE_REPRESENTATION(#102,#11894);
#164=CONTEXT_DEPENDENT_SHAPE_REPRESENTATION(#103,#11895);
#165=CONTEXT_DEPENDENT_SHAPE_REPRESENTATION(#104,#11896);
#166=CONTEXT_DEPENDENT_SHAPE_REPRESENTATION(#105,#11897);
#167=CONTEXT_DEPENDENT_SHAPE_REPRESENTATION(#106,#11898);
#168=CONTEXT_DEPENDENT_SHAPE_REPRESENTATION(#107,#11899);
#169=CONTEXT_DEPENDENT_SHAPE_REPRESENTATION(#108,#11900);
#170=CONTEXT_DEPENDENT_SHAPE_REPRESENTATION(#109,#11901);
#171=CONTEXT_DEPENDENT_SHAPE_REPRESENTATION(#110,#11902);
#172=CONTEXT_DEPENDENT_SHAPE_REPRESENTATION(#111,#11903);
#173=CONTEXT_DEPENDENT_SHAPE_REPRESENTATION(#112,#11904);
#174=CONTEXT_DEPENDENT_SHAPE_REPRESENTATION(#113,#11905);
#175=CONTEXT_DEPENDENT_SHAPE_REPRESENTATION(#114,#11906);
#176=CONTEXT_DEPENDENT_SHAPE_REPRESENTATION(#115,#11907);
#177=CONTEXT_DEPENDENT_SHAPE_REPRESENTATION(#116,#11908);
#178=CONTEXT_DEPENDENT_SHAPE_REPRESENTATION(#117,#11909);
#179=CONTEXT_DEPENDENT_SHAPE_REPRESENTATION(#118,#11910);
#180=CONTEXT_DEPENDENT_SHAPE_REPRESENTATION(#119,#11911);
#181=CONTEXT_DEPENDENT_SHAPE_REPRESENTATION(#120,#11912);
#182=CONTEXT_DEPENDENT_SHAPE_REPRESENTATION(#121,#11913);
#183=CONTEXT_DEPENDENT_SHAPE_REPRESENTATION(#122,#11914);
#184=CONTEXT_DEPENDENT_SHAPE_REPRESENTATION(#123,#11915);
#185=CONTEXT_DEPENDENT_SHAPE_REPRESENTATION(#124,#11916);
#186=CONTEXT_DEPENDENT_SHAPE_REPRESENTATION(#125,#11917);
#187=CONTEXT_DEPENDENT_SHAPE_REPRESENTATION(#126,#11918);
#188=CONTEXT_DEPENDENT_SHAPE_REPRESENTATION(#127,#11919);
#189=CONTEXT_DEPENDENT_SHAPE_REPRESENTATION(#128,#11920);
#190=CONTEXT_DEPENDENT_SHAPE_REPRESENTATION(#129,#11921);
#191=CONTEXT_DEPENDENT_SHAPE_REPRESENTATION(#130,#11922);
#192=CONTEXT_DEPENDENT_SHAPE_REPRESENTATION(#131,#11923);
#193=CONTEXT_DEPENDENT_SHAPE_REPRESENTATION(#132,#11924);
#194=CONTEXT_DEPENDENT_SHAPE_REPRESENTATION(#133,#11925);
#195=CONTEXT_DEPENDENT_SHAPE_REPRESENTATION(#134,#11926);
#196=CONTEXT_DEPENDENT_SHAPE_REPRESENTATION(#135,#11927);
#197=CONTEXT_DEPENDENT_SHAPE_REPRESENTATION(#136,#11928);
#198=CONTEXT_DEPENDENT_SHAPE_REPRESENTATION(#137,#11929);
#199=CONTEXT_DEPENDENT_SHAPE_REPRESENTATION(#138,#11930);
#200=CONTEXT_DEPENDENT_SHAPE_REPRESENTATION(#139,#11931);
#201=CONTEXT_DEPENDENT_SHAPE_REPRESENTATION(#140,#11932);
#202=CONTEXT_DEPENDENT_SHAPE_REPRESENTATION(#141,#11933);
#203=CONTEXT_DEPENDENT_SHAPE_REPRESENTATION(#142,#11934);
#204=CONTEXT_DEPENDENT_SHAPE_REPRESENTATION(#143,#11935);
#205=CONTEXT_DEPENDENT_SHAPE_REPRESENTATION(#144,#11936);
#206=CONTEXT_DEPENDENT_SHAPE_REPRESENTATION(#145,#11937);
#207=CONTEXT_DEPENDENT_SHAPE_REPRESENTATION(#146,#11938);
#208=CONTEXT_DEPENDENT_SHAPE_REPRESENTATION(#147,#11941);
#209=CONTEXT_DEPENDENT_SHAPE_REPRESENTATION(#148,#11942);
#210=CONTEXT_DEPENDENT_SHAPE_REPRESENTATION(#149,#11943);
#211=CONTEXT_DEPENDENT_SHAPE_REPRESENTATION(#150,#11944);
#212=NEXT_ASSEMBLY_USAGE_OCCURRENCE('Housing:1','Housing:1','Housing:1',
#12002,#12003,'Housing:1');
#213=NEXT_ASSEMBLY_USAGE_OCCURRENCE('Insert bearing:1',
'Insert bearing:1','Insert bearing:1',#12002,#12004,'Insert bearing:1');
#214=NEXT_ASSEMBLY_USAGE_OCCURRENCE('Base:1','Base:1','Base:1',#11986,#11987,
'Base:1');
#215=NEXT_ASSEMBLY_USAGE_OCCURRENCE('Foot:1','Foot:1','Foot:1',#11986,#11988,
'Foot:1');
#216=NEXT_ASSEMBLY_USAGE_OCCURRENCE('Foot (1):1','Foot (1):1',
'Foot (1):1',#11986,#11989,'Foot (1):1');
#217=NEXT_ASSEMBLY_USAGE_OCCURRENCE('Bearing riser:1','Bearing riser:1',
'Bearing riser:1',#11986,#11990,'Bearing riser:1');
#218=NEXT_ASSEMBLY_USAGE_OCCURRENCE('Mounting bush:1','Mounting bush:1',
'Mounting bush:1',#11986,#11991,'Mounting bush:1');
#219=NEXT_ASSEMBLY_USAGE_OCCURRENCE('Mounting bush (1):1',
'Mounting bush (1):1','Mounting bush (1):1',#11986,#11992,
'Mounting bush (1):1');
#220=NEXT_ASSEMBLY_USAGE_OCCURRENCE('Bearing riser (1):1',
'Bearing riser (1):1','Bearing riser (1):1',#11986,#11993,
'Bearing riser (1):1');
#221=NEXT_ASSEMBLY_USAGE_OCCURRENCE('Mounting bush (2):1',
'Mounting bush (2):1','Mounting bush (2):1',#11986,#11994,
'Mounting bush (2):1');
#222=NEXT_ASSEMBLY_USAGE_OCCURRENCE('Mounting bush (3):1',
'Mounting bush (3):1','Mounting bush (3):1',#11986,#11995,
'Mounting bush (3):1');
#223=NEXT_ASSEMBLY_USAGE_OCCURRENCE('Pawl pedestal:1','Pawl pedestal:1',
'Pawl pedestal:1',#11986,#11996,'Pawl pedestal:1');
#224=NEXT_ASSEMBLY_USAGE_OCCURRENCE('Pawl pivot pin:1',
'Pawl pivot pin:1','Pawl pivot pin:1',#11986,#11997,'Pawl pivot pin:1');
#225=NEXT_ASSEMBLY_USAGE_OCCURRENCE('Pawl pivot sleeve:1',
'Pawl pivot sleeve:1','Pawl pivot sleeve:1',#11986,#11998,
'Pawl pivot sleeve:1');
#226=NEXT_ASSEMBLY_USAGE_OCCURRENCE('Pawl pin keeper:1',
'Pawl pin keeper:1','Pawl pin keeper:1',#11986,#11999,
'Pawl pin keeper:1');
#227=NEXT_ASSEMBLY_USAGE_OCCURRENCE('Pawl leaf spring:1',
'Pawl leaf spring:1','Pawl leaf spring:1',#11986,#12000,
'Pawl leaf spring:1');
#228=NEXT_ASSEMBLY_USAGE_OCCURRENCE('Spring anchor:1','Spring anchor:1',
'Spring anchor:1',#11986,#12001,'Spring anchor:1');
#229=NEXT_ASSEMBLY_USAGE_OCCURRENCE('Cap Screw - M5x20:2',
'Cap Screw - M5x20:2','Cap Screw - M5x20:2',#11986,#12021,
'Cap Screw - M5x20:2');
#230=NEXT_ASSEMBLY_USAGE_OCCURRENCE('Cap Screw - M5x20:3',
'Cap Screw - M5x20:3','Cap Screw - M5x20:3',#11986,#12021,
'Cap Screw - M5x20:3');
#231=NEXT_ASSEMBLY_USAGE_OCCURRENCE('Cap Screw - M5x20:4',
'Cap Screw - M5x20:4','Cap Screw - M5x20:4',#11986,#12021,
'Cap Screw - M5x20:4');
#232=NEXT_ASSEMBLY_USAGE_OCCURRENCE('Cap Screw - M5x20:5',
'Cap Screw - M5x20:5','Cap Screw - M5x20:5',#11986,#12021,
'Cap Screw - M5x20:5');
#233=NEXT_ASSEMBLY_USAGE_OCCURRENCE(
'Pillow Block Bearing - 20 mm Bore:2',
'Pillow Block Bearing - 20 mm Bore:2',
'Pillow Block Bearing - 20 mm Bore:2',#11986,#12002,
'Pillow Block Bearing - 20 mm Bore:2');
#234=NEXT_ASSEMBLY_USAGE_OCCURRENCE('Flat Washer - M8:2',
'Flat Washer - M8:2','Flat Washer - M8:2',#11986,#12005,
'Flat Washer - M8:2');
#235=NEXT_ASSEMBLY_USAGE_OCCURRENCE('M8x25 Bolt:2','M8x25 Bolt:2',
'M8x25 Bolt:2',#11986,#12006,'M8x25 Bolt:2');
#236=NEXT_ASSEMBLY_USAGE_OCCURRENCE('Flat Washer - M8:3',
'Flat Washer - M8:3','Flat Washer - M8:3',#11986,#12005,
'Flat Washer - M8:3');
#237=NEXT_ASSEMBLY_USAGE_OCCURRENCE('M8x25 Bolt:3','M8x25 Bolt:3',
'M8x25 Bolt:3',#11986,#12006,'M8x25 Bolt:3');
#238=NEXT_ASSEMBLY_USAGE_OCCURRENCE('Cap Screw - M5x20:6',
'Cap Screw - M5x20:6','Cap Screw - M5x20:6',#11986,#12021,
'Cap Screw - M5x20:6');
#239=NEXT_ASSEMBLY_USAGE_OCCURRENCE('Cap Screw - M5x20:7',
'Cap Screw - M5x20:7','Cap Screw - M5x20:7',#11986,#12021,
'Cap Screw - M5x20:7');
#240=NEXT_ASSEMBLY_USAGE_OCCURRENCE('Cap Screw - M5x20:8',
'Cap Screw - M5x20:8','Cap Screw - M5x20:8',#11986,#12021,
'Cap Screw - M5x20:8');
#241=NEXT_ASSEMBLY_USAGE_OCCURRENCE('Cap Screw - M5x20:9',
'Cap Screw - M5x20:9','Cap Screw - M5x20:9',#11986,#12021,
'Cap Screw - M5x20:9');
#242=NEXT_ASSEMBLY_USAGE_OCCURRENCE(
'Pillow Block Bearing - 20 mm Bore:3',
'Pillow Block Bearing - 20 mm Bore:3',
'Pillow Block Bearing - 20 mm Bore:3',#11986,#12002,
'Pillow Block Bearing - 20 mm Bore:3');
#243=NEXT_ASSEMBLY_USAGE_OCCURRENCE('Flat Washer - M8:4',
'Flat Washer - M8:4','Flat Washer - M8:4',#11986,#12005,
'Flat Washer - M8:4');
#244=NEXT_ASSEMBLY_USAGE_OCCURRENCE('M8x25 Bolt:4','M8x25 Bolt:4',
'M8x25 Bolt:4',#11986,#12006,'M8x25 Bolt:4');
#245=NEXT_ASSEMBLY_USAGE_OCCURRENCE('Flat Washer - M8:5',
'Flat Washer - M8:5','Flat Washer - M8:5',#11986,#12005,
'Flat Washer - M8:5');
#246=NEXT_ASSEMBLY_USAGE_OCCURRENCE('M8x25 Bolt:5','M8x25 Bolt:5',
'M8x25 Bolt:5',#11986,#12006,'M8x25 Bolt:5');
#247=NEXT_ASSEMBLY_USAGE_OCCURRENCE('Cap Screw - M5x20:11',
'Cap Screw - M5x20:11','Cap Screw - M5x20:11',#11986,#12021,
'Cap Screw - M5x20:11');
#248=NEXT_ASSEMBLY_USAGE_OCCURRENCE('Cap Screw - M5x20:12',
'Cap Screw - M5x20:12','Cap Screw - M5x20:12',#11986,#12021,
'Cap Screw - M5x20:12');
#249=NEXT_ASSEMBLY_USAGE_OCCURRENCE('M4x10 Cap Screw:2',
'M4x10 Cap Screw:2','M4x10 Cap Screw:2',#11986,#12007,
'M4x10 Cap Screw:2');
#250=NEXT_ASSEMBLY_USAGE_OCCURRENCE('M4x10 Cap Screw:3',
'M4x10 Cap Screw:3','M4x10 Cap Screw:3',#11986,#12007,
'M4x10 Cap Screw:3');
#251=NEXT_ASSEMBLY_USAGE_OCCURRENCE('Drum shaft:1','Drum shaft:1',
'Drum shaft:1',#12008,#12009,'Drum shaft:1');
#252=NEXT_ASSEMBLY_USAGE_OCCURRENCE('Shaft collar:1','Shaft collar:1',
'Shaft collar:1',#12008,#12010,'Shaft collar:1');
#253=NEXT_ASSEMBLY_USAGE_OCCURRENCE('Shaft collar (1):1',
'Shaft collar (1):1','Shaft collar (1):1',#12008,#12011,
'Shaft collar (1):1');
#254=NEXT_ASSEMBLY_USAGE_OCCURRENCE('Winding drum:1','Winding drum:1',
'Winding drum:1',#12008,#12012,'Winding drum:1');
#255=NEXT_ASSEMBLY_USAGE_OCCURRENCE('Drum flange:1','Drum flange:1',
'Drum flange:1',#12008,#12013,'Drum flange:1');
#256=NEXT_ASSEMBLY_USAGE_OCCURRENCE('Drum hub:1','Drum hub:1',
'Drum hub:1',#12008,#12014,'Drum hub:1');
#257=NEXT_ASSEMBLY_USAGE_OCCURRENCE('Drum flange (1):1',
'Drum flange (1):1','Drum flange (1):1',#12008,#12015,
'Drum flange (1):1');
#258=NEXT_ASSEMBLY_USAGE_OCCURRENCE('Drum hub (1):1','Drum hub (1):1',
'Drum hub (1):1',#12008,#12016,'Drum hub (1):1');
#259=NEXT_ASSEMBLY_USAGE_OCCURRENCE('Ratchet wheel:1','Ratchet wheel:1',
'Ratchet wheel:1',#12008,#12017,'Ratchet wheel:1');
#260=NEXT_ASSEMBLY_USAGE_OCCURRENCE('Crank:1','Crank:1','Crank:1',#12008,
#12018,'Crank:1');
#261=NEXT_ASSEMBLY_USAGE_OCCURRENCE('Handle:1','Handle:1','Handle:1',#12008,
#12019,'Handle:1');
#262=NEXT_ASSEMBLY_USAGE_OCCURRENCE('Socket Set Screw - M5x8:2',
'Socket Set Screw - M5x8:2','Socket Set Screw - M5x8:2',#12008,#12020,
'Socket Set Screw - M5x8:2');
#263=NEXT_ASSEMBLY_USAGE_OCCURRENCE('Socket Set Screw - M5x8:3',
'Socket Set Screw - M5x8:3','Socket Set Screw - M5x8:3',#12008,#12020,
'Socket Set Screw - M5x8:3');
#264=NEXT_ASSEMBLY_USAGE_OCCURRENCE('Socket Set Screw - M5x8:4',
'Socket Set Screw - M5x8:4','Socket Set Screw - M5x8:4',#12008,#12020,
'Socket Set Screw - M5x8:4');
#265=NEXT_ASSEMBLY_USAGE_OCCURRENCE('Socket Set Screw - M5x8:5',
'Socket Set Screw - M5x8:5','Socket Set Screw - M5x8:5',#12008,#12020,
'Socket Set Screw - M5x8:5');
#266=NEXT_ASSEMBLY_USAGE_OCCURRENCE('Socket Set Screw - M5x8:6',
'Socket Set Screw - M5x8:6','Socket Set Screw - M5x8:6',#12008,#12020,
'Socket Set Screw - M5x8:6');
#267=NEXT_ASSEMBLY_USAGE_OCCURRENCE('Socket Set Screw - M5x8:7',
'Socket Set Screw - M5x8:7','Socket Set Screw - M5x8:7',#12008,#12020,
'Socket Set Screw - M5x8:7');
#268=NEXT_ASSEMBLY_USAGE_OCCURRENCE('Cap Screw - M5x20:10',
'Cap Screw - M5x20:10','Cap Screw - M5x20:10',#12008,#12021,
'Cap Screw - M5x20:10');
#269=NEXT_ASSEMBLY_USAGE_OCCURRENCE('Pawl (1):1','Pawl (1):1',
'Pawl (1):1',#12022,#12023,'Pawl (1):1');
#270=NEXT_ASSEMBLY_USAGE_OCCURRENCE('Base and bearing supports:1',
'Base and bearing supports:1','Base and bearing supports:1',#11985,#11986,
'Base and bearing supports:1');
#271=NEXT_ASSEMBLY_USAGE_OCCURRENCE('Drum shaft and crank:1',
'Drum shaft and crank:1','Drum shaft and crank:1',#11985,#12008,
'Drum shaft and crank:1');
#272=NEXT_ASSEMBLY_USAGE_OCCURRENCE('Pawl:1','Pawl:1','Pawl:1',#11985,#12022,
'Pawl:1');
#273=B_SPLINE_CURVE_WITH_KNOTS('',3,(#9945,#9946,#9947,#9948,#9949,#9950,
#9951,#9952,#9953,#9954),.UNSPECIFIED.,.F.,.F.,(4,2,2,2,4),(1.13193471301885,
1.22626174930539,1.32058878559194,1.41491753480854,1.50924628402513),
 .UNSPECIFIED.);
#274=B_SPLINE_CURVE_WITH_KNOTS('',3,(#9956,#9957,#9958,#9959,#9960,#9961,
#9962,#9963,#9964,#9965,#9966,#9967,#9968,#9969,#9970,#9971,#9972,#9973),
 .UNSPECIFIED.,.F.,.F.,(4,2,2,2,2,2,2,2,4),(0.377311571006283,0.471638607292829,
0.565965643579376,0.66029439279597,0.754623142012565,0.84895189122916,0.943280640445754,
1.0376076767323,1.13193471301885),.UNSPECIFIED.);
#275=B_SPLINE_CURVE_WITH_KNOTS('',3,(#9974,#9975,#9976,#9977,#9978,#9979,
#9980,#9981,#9982,#9983),.UNSPECIFIED.,.F.,.F.,(4,2,2,2,4),(1.50924628402513,
1.60357503324173,1.69790378245832,1.79223081874487,1.88655785503141),
 .UNSPECIFIED.);
#276=B_SPLINE_CURVE_WITH_KNOTS('',3,(#9986,#9987,#9988,#9989,#9990,#9991,
#9992,#9993,#9994,#9995,#9996,#9997,#9998,#9999,#10000,#10001,#10002,#10003,
#10004,#10005,#10006,#10007,#10008,#10009,#10010,#10011,#10012,#10013,#10014,
#10015,#10016,#10017,#10018,#10019),.UNSPECIFIED.,.T.,.F.,(4,2,2,2,2,2,
2,2,2,2,2,2,2,2,2,2,4),(0.,0.0946120580087934,0.189224116017587,0.283822945575014,
0.378421775132442,0.47302060468987,0.567619434247297,0.662231492256091,
0.756843550264884,0.851455608273677,0.94606766628247,1.0406664958399,1.13526532539733,
1.22986415495475,1.32446298451218,1.41907504252097,1.51368710052977),
 .UNSPECIFIED.);
#277=B_SPLINE_CURVE_WITH_KNOTS('',3,(#10022,#10023,#10024,#10025,#10026,
#10027,#10028,#10029,#10030,#10031,#10032,#10033,#10034,#10035,#10036,#10037,
#10038,#10039,#10040,#10041,#10042,#10043,#10044,#10045,#10046,#10047,#10048,
#10049,#10050,#10051,#10052,#10053,#10054,#10055),.UNSPECIFIED.,.T.,.F.,
(4,2,2,2,2,2,2,2,2,2,2,2,2,2,2,2,4),(0.,0.0946120580087934,0.189224116017587,
0.283822945575014,0.378421775132442,0.47302060468987,0.567619434247297,
0.66223149225609,0.756843550264884,0.851455608273677,0.94606766628247,1.0406664958399,
1.13526532539733,1.22986415495475,1.32446298451218,1.41907504252097,1.51368710052977),
 .UNSPECIFIED.);
#278=B_SPLINE_CURVE_WITH_KNOTS('',3,(#10059,#10060,#10061,#10062,#10063,
#10064,#10065,#10066,#10067,#10068),.UNSPECIFIED.,.F.,.F.,(4,2,2,2,4),(1.13193471301885,
1.22626174930539,1.32058878559194,1.41491753480854,1.50924628402513),
 .UNSPECIFIED.);
#279=B_SPLINE_CURVE_WITH_KNOTS('',3,(#10070,#10071,#10072,#10073,#10074,
#10075,#10076,#10077,#10078,#10079,#10080,#10081,#10082,#10083,#10084,#10085,
#10086,#10087),.UNSPECIFIED.,.F.,.F.,(4,2,2,2,2,2,2,2,4),(0.377311571006283,
0.47163860729283,0.565965643579376,0.660294392795971,0.754623142012565,
0.84895189122916,0.943280640445755,1.0376076767323,1.13193471301885),
 .UNSPECIFIED.);
#280=B_SPLINE_CURVE_WITH_KNOTS('',3,(#10088,#10089,#10090,#10091,#10092,
#10093,#10094,#10095,#10096,#10097),.UNSPECIFIED.,.F.,.F.,(4,2,2,2,4),(1.50924628402513,
1.60357503324173,1.69790378245832,1.79223081874487,1.88655785503141),
 .UNSPECIFIED.);
#281=B_SPLINE_CURVE_WITH_KNOTS('',3,(#10106,#10107,#10108,#10109,#10110,
#10111,#10112,#10113,#10114,#10115,#10116,#10117,#10118,#10119,#10120,#10121,
#10122,#10123),.UNSPECIFIED.,.F.,.F.,(4,2,2,2,2,2,2,2,4),(0.377311571006282,
0.471638607292829,0.565965643579376,0.660294392795971,0.754623142012565,
0.84895189122916,0.943280640445754,1.0376076767323,1.13193471301885),
 .UNSPECIFIED.);
#282=B_SPLINE_CURVE_WITH_KNOTS('',3,(#10125,#10126,#10127,#10128,#10129,
#10130,#10131,#10132,#10133,#10134),.UNSPECIFIED.,.F.,.F.,(4,2,2,2,4),(1.13193471301885,
1.22626174930539,1.32058878559194,1.41491753480854,1.50924628402513),
 .UNSPECIFIED.);
#283=B_SPLINE_CURVE_WITH_KNOTS('',3,(#10135,#10136,#10137,#10138,#10139,
#10140,#10141,#10142,#10143,#10144),.UNSPECIFIED.,.F.,.F.,(4,2,2,2,4),(1.50924628402513,
1.60357503324172,1.69790378245832,1.79223081874487,1.88655785503141),
 .UNSPECIFIED.);
#284=B_SPLINE_CURVE_WITH_KNOTS('',3,(#10147,#10148,#10149,#10150,#10151,
#10152,#10153,#10154,#10155,#10156,#10157,#10158,#10159,#10160,#10161,#10162,
#10163,#10164),.UNSPECIFIED.,.F.,.F.,(4,2,2,2,2,2,2,2,4),(0.377311571006283,
0.47163860729283,0.565965643579376,0.660294392795971,0.754623142012565,
0.84895189122916,0.943280640445754,1.0376076767323,1.13193471301885),
 .UNSPECIFIED.);
#285=B_SPLINE_CURVE_WITH_KNOTS('',3,(#10166,#10167,#10168,#10169,#10170,
#10171,#10172,#10173,#10174,#10175),.UNSPECIFIED.,.F.,.F.,(4,2,2,2,4),(1.13193471301885,
1.22626174930539,1.32058878559194,1.41491753480854,1.50924628402513),
 .UNSPECIFIED.);
#286=B_SPLINE_CURVE_WITH_KNOTS('',3,(#10176,#10177,#10178,#10179,#10180,
#10181,#10182,#10183,#10184,#10185),.UNSPECIFIED.,.F.,.F.,(4,2,2,2,4),(1.50924628402513,
1.60357503324173,1.69790378245832,1.79223081874487,1.88655785503141),
 .UNSPECIFIED.);
#287=B_SPLINE_CURVE_WITH_KNOTS('',3,(#10188,#10189,#10190,#10191,#10192,
#10193,#10194,#10195,#10196,#10197,#10198,#10199,#10200,#10201,#10202,#10203,
#10204,#10205),.UNSPECIFIED.,.F.,.F.,(4,2,2,2,2,2,2,2,4),(0.377311571006282,
0.471638607292829,0.565965643579376,0.66029439279597,0.754623142012565,
0.84895189122916,0.943280640445754,1.0376076767323,1.13193471301885),
 .UNSPECIFIED.);
#288=B_SPLINE_CURVE_WITH_KNOTS('',3,(#10207,#10208,#10209,#10210,#10211,
#10212,#10213,#10214,#10215,#10216),.UNSPECIFIED.,.F.,.F.,(4,2,2,2,4),(1.13193471301885,
1.22626174930539,1.32058878559194,1.41491753480854,1.50924628402513),
 .UNSPECIFIED.);
#289=B_SPLINE_CURVE_WITH_KNOTS('',3,(#10217,#10218,#10219,#10220,#10221,
#10222,#10223,#10224,#10225,#10226),.UNSPECIFIED.,.F.,.F.,(4,2,2,2,4),(1.50924628402513,
1.60357503324172,1.69790378245832,1.79223081874487,1.88655785503141),
 .UNSPECIFIED.);
#290=B_SPLINE_CURVE_WITH_KNOTS('',3,(#10229,#10230,#10231,#10232,#10233,
#10234,#10235,#10236,#10237,#10238,#10239,#10240,#10241,#10242,#10243,#10244,
#10245,#10246),.UNSPECIFIED.,.F.,.F.,(4,2,2,2,2,2,2,2,4),(0.377311571006283,
0.471638607292829,0.565965643579376,0.660294392795971,0.754623142012565,
0.84895189122916,0.943280640445755,1.0376076767323,1.13193471301885),
 .UNSPECIFIED.);
#291=B_SPLINE_CURVE_WITH_KNOTS('',3,(#10248,#10249,#10250,#10251,#10252,
#10253,#10254,#10255,#10256,#10257),.UNSPECIFIED.,.F.,.F.,(4,2,2,2,4),(1.13193471301885,
1.22626174930539,1.32058878559194,1.41491753480854,1.50924628402513),
 .UNSPECIFIED.);
#292=B_SPLINE_CURVE_WITH_KNOTS('',3,(#10258,#10259,#10260,#10261,#10262,
#10263,#10264,#10265,#10266,#10267),.UNSPECIFIED.,.F.,.F.,(4,2,2,2,4),(1.50924628402513,
1.60357503324172,1.69790378245832,1.79223081874487,1.88655785503141),
 .UNSPECIFIED.);
#293=B_SPLINE_CURVE_WITH_KNOTS('',3,(#10271,#10272,#10273,#10274,#10275,
#10276,#10277,#10278,#10279,#10280,#10281,#10282,#10283,#10284,#10285,#10286,
#10287,#10288,#10289,#10290,#10291,#10292,#10293,#10294,#10295,#10296,#10297,
#10298,#10299,#10300,#10301,#10302,#10303,#10304),.UNSPECIFIED.,.T.,.F.,
(4,2,2,2,2,2,2,2,2,2,2,2,2,2,2,2,4),(0.,0.0946120580087934,0.189224116017587,
0.283822945575014,0.378421775132442,0.47302060468987,0.567619434247297,
0.66223149225609,0.756843550264884,0.851455608273677,0.94606766628247,1.0406664958399,
1.13526532539733,1.22986415495475,1.32446298451218,1.41907504252097,1.51368710052977),
 .UNSPECIFIED.);
#294=B_SPLINE_CURVE_WITH_KNOTS('',3,(#10307,#10308,#10309,#10310,#10311,
#10312,#10313,#10314,#10315,#10316,#10317,#10318,#10319,#10320,#10321,#10322,
#10323,#10324,#10325,#10326,#10327,#10328,#10329,#10330,#10331,#10332,#10333,
#10334,#10335,#10336,#10337,#10338,#10339,#10340),.UNSPECIFIED.,.T.,.F.,
(4,2,2,2,2,2,2,2,2,2,2,2,2,2,2,2,4),(0.,0.0946120580087934,0.189224116017587,
0.283822945575014,0.378421775132442,0.47302060468987,0.567619434247297,
0.66223149225609,0.756843550264884,0.851455608273677,0.94606766628247,1.0406664958399,
1.13526532539733,1.22986415495475,1.32446298451218,1.41907504252097,1.51368710052977),
 .UNSPECIFIED.);
#295=B_SPLINE_CURVE_WITH_KNOTS('',3,(#10345,#10346,#10347,#10348,#10349,
#10350,#10351,#10352,#10353,#10354,#10355,#10356,#10357,#10358,#10359,#10360,
#10361,#10362,#10363,#10364,#10365,#10366,#10367,#10368,#10369,#10370,#10371,
#10372,#10373,#10374,#10375,#10376,#10377,#10378),.UNSPECIFIED.,.T.,.F.,
(4,2,2,2,2,2,2,2,2,2,2,2,2,2,2,2,4),(0.,0.0946120580087934,0.189224116017587,
0.283822945575014,0.378421775132442,0.47302060468987,0.567619434247297,
0.66223149225609,0.756843550264884,0.851455608273677,0.94606766628247,1.0406664958399,
1.13526532539733,1.22986415495475,1.32446298451218,1.41907504252097,1.51368710052977),
 .UNSPECIFIED.);
#296=B_SPLINE_CURVE_WITH_KNOTS('',3,(#10381,#10382,#10383,#10384,#10385,
#10386,#10387,#10388,#10389,#10390,#10391,#10392,#10393,#10394,#10395,#10396,
#10397,#10398,#10399,#10400,#10401,#10402,#10403,#10404,#10405,#10406,#10407,
#10408,#10409,#10410,#10411,#10412,#10413,#10414),.UNSPECIFIED.,.T.,.F.,
(4,2,2,2,2,2,2,2,2,2,2,2,2,2,2,2,4),(0.,0.0946120580087934,0.189224116017587,
0.283822945575014,0.378421775132442,0.47302060468987,0.567619434247297,
0.66223149225609,0.756843550264884,0.851455608273677,0.94606766628247,1.0406664958399,
1.13526532539733,1.22986415495475,1.32446298451218,1.41907504252097,1.51368710052977),
 .UNSPECIFIED.);
#297=B_SPLINE_CURVE_WITH_KNOTS('',3,(#10598,#10599,#10600,#10601,#10602,
#10603,#10604,#10605,#10606,#10607,#10608,#10609,#10610,#10611),
 .UNSPECIFIED.,.F.,.F.,(4,2,2,2,2,2,4),(0.75600573798702,0.793568827564647,
0.872922520054201,0.952276212543756,1.03162990503331,1.11098359752287,1.14854668710049),
 .UNSPECIFIED.);
#298=B_SPLINE_CURVE_WITH_KNOTS('',3,(#10617,#10618,#10619,#10620,#10621,
#10622,#10623,#10624,#10625,#10626,#10627,#10628,#10629,#10630,#10631,#10632,
#10633,#10634),.UNSPECIFIED.,.F.,.F.,(4,2,2,2,2,2,2,2,4),(0.,0.079216580773363,
0.158433161546726,0.23764869707457,0.316864232602414,0.396079768130259,
0.475295303658103,0.554511884431466,0.633728465204829),.UNSPECIFIED.);
#299=B_SPLINE_CURVE_WITH_KNOTS('',3,(#10635,#10636,#10637,#10638,#10639,
#10640,#10641,#10642,#10643,#10644,#10645,#10646,#10647,#10648,#10649,#10650,
#10651,#10652),.UNSPECIFIED.,.F.,.F.,(4,2,2,2,2,2,2,2,4),(0.633728465204829,
0.712945045978192,0.792161626751555,0.871377162279399,0.950592697807243,
1.02980823333509,1.10902376886293,1.18824034963629,1.26745693040966),
 .UNSPECIFIED.);
#300=B_SPLINE_CURVE_WITH_KNOTS('',3,(#10655,#10656,#10657,#10658,#10659,
#10660,#10661,#10662,#10663,#10664,#10665,#10666,#10667,#10668),
 .UNSPECIFIED.,.F.,.F.,(4,2,2,2,2,2,4),(0.121154929624515,0.158718019202143,
0.238071711691697,0.317425404181252,0.396779096670807,0.476132789160362,
0.513695878737989),.UNSPECIFIED.);
#301=B_SPLINE_CURVE_WITH_KNOTS('',3,(#10693,#10694,#10695,#10696,#10697,
#10698,#10699,#10700,#10701,#10702,#10703,#10704,#10705,#10706),
 .UNSPECIFIED.,.F.,.F.,(4,2,2,2,2,2,4),(0.756005737987024,0.793568827564645,
0.8729225200542,0.952276212543755,1.03162990503331,1.11098359752287,1.14854668710049),
 .UNSPECIFIED.);
#302=B_SPLINE_CURVE_WITH_KNOTS('',3,(#10712,#10713,#10714,#10715,#10716,
#10717,#10718,#10719,#10720,#10721,#10722,#10723,#10724,#10725,#10726,#10727,
#10728,#10729),.UNSPECIFIED.,.F.,.F.,(4,2,2,2,2,2,2,2,4),(0.,0.0792165807733624,
0.158433161546725,0.23764869707457,0.316864232602414,0.396079768130259,
0.475295303658103,0.554511884431466,0.633728465204828),.UNSPECIFIED.);
#303=B_SPLINE_CURVE_WITH_KNOTS('',3,(#10730,#10731,#10732,#10733,#10734,
#10735,#10736,#10737,#10738,#10739,#10740,#10741,#10742,#10743,#10744,#10745,
#10746,#10747),.UNSPECIFIED.,.F.,.F.,(4,2,2,2,2,2,2,2,4),(0.633728465204828,
0.712945045978191,0.792161626751553,0.871377162279398,0.950592697807242,
1.02980823333509,1.10902376886293,1.18824034963629,1.26745693040966),
 .UNSPECIFIED.);
#304=B_SPLINE_CURVE_WITH_KNOTS('',3,(#10750,#10751,#10752,#10753,#10754,
#10755,#10756,#10757,#10758,#10759,#10760,#10761,#10762,#10763),
 .UNSPECIFIED.,.F.,.F.,(4,2,2,2,2,2,4),(0.121154929624523,0.158718019202141,
0.238071711691696,0.317425404181252,0.396779096670807,0.476132789160362,
0.51369587873798),.UNSPECIFIED.);
#305=B_SPLINE_CURVE_WITH_KNOTS('',3,(#10818,#10819,#10820,#10821,#10822,
#10823,#10824,#10825,#10826,#10827,#10828,#10829,#10830,#10831),
 .UNSPECIFIED.,.F.,.F.,(4,2,2,2,2,2,4),(0.756005737987019,0.793568827564647,
0.872922520054201,0.952276212543756,1.03162990503331,1.11098359752287,1.14854668710049),
 .UNSPECIFIED.);
#306=B_SPLINE_CURVE_WITH_KNOTS('',3,(#10837,#10838,#10839,#10840,#10841,
#10842,#10843,#10844,#10845,#10846,#10847,#10848,#10849,#10850,#10851,#10852,
#10853,#10854),.UNSPECIFIED.,.F.,.F.,(4,2,2,2,2,2,2,2,4),(0.,0.0792028026112439,
0.158405605222488,0.237607602356377,0.316809599490267,0.396011596624156,
0.475213593758045,0.554416396369289,0.633619198980533),.UNSPECIFIED.);
#307=B_SPLINE_CURVE_WITH_KNOTS('',3,(#10855,#10856,#10857,#10858,#10859,
#10860,#10861,#10862,#10863,#10864,#10865,#10866,#10867,#10868,#10869,#10870,
#10871,#10872),.UNSPECIFIED.,.F.,.F.,(4,2,2,2,2,2,2,2,4),(0.633619198980533,
0.712822001591777,0.792024804203021,0.87122680133691,0.950428798470799,
1.02963079560469,1.10883279273858,1.18803559534982,1.26723839796107),
 .UNSPECIFIED.);
#308=B_SPLINE_CURVE_WITH_KNOTS('',3,(#10875,#10876,#10877,#10878,#10879,
#10880,#10881,#10882,#10883,#10884,#10885,#10886,#10887,#10888),
 .UNSPECIFIED.,.F.,.F.,(4,2,2,2,2,2,4),(0.121154929624516,0.158718019202143,
0.238071711691697,0.317425404181252,0.396779096670807,0.476132789160362,
0.513695878737988),.UNSPECIFIED.);
#309=B_SPLINE_CURVE_WITH_KNOTS('',3,(#10928,#10929,#10930,#10931,#10932,
#10933,#10934,#10935,#10936,#10937,#10938,#10939,#10940,#10941),
 .UNSPECIFIED.,.F.,.F.,(4,2,2,2,2,2,4),(0.756005737987023,0.793568827564648,
0.872922520054203,0.952276212543758,1.03162990503331,1.11098359752287,1.1485466871005),
 .UNSPECIFIED.);
#310=B_SPLINE_CURVE_WITH_KNOTS('',3,(#10947,#10948,#10949,#10950,#10951,
#10952,#10953,#10954,#10955,#10956,#10957,#10958,#10959,#10960,#10961,#10962,
#10963,#10964),.UNSPECIFIED.,.F.,.F.,(4,2,2,2,2,2,2,2,4),(0.,0.0792028026112442,
0.158405605222488,0.237607602356378,0.316809599490267,0.396011596624156,
0.475213593758046,0.55441639636929,0.633619198980534),.UNSPECIFIED.);
#311=B_SPLINE_CURVE_WITH_KNOTS('',3,(#10965,#10966,#10967,#10968,#10969,
#10970,#10971,#10972,#10973,#10974,#10975,#10976,#10977,#10978,#10979,#10980,
#10981,#10982),.UNSPECIFIED.,.F.,.F.,(4,2,2,2,2,2,2,2,4),(0.633619198980534,
0.712822001591778,0.792024804203022,0.871226801336912,0.950428798470801,
1.02963079560469,1.10883279273858,1.18803559534982,1.26723839796107),
 .UNSPECIFIED.);
#312=B_SPLINE_CURVE_WITH_KNOTS('',3,(#10985,#10986,#10987,#10988,#10989,
#10990,#10991,#10992,#10993,#10994,#10995,#10996,#10997,#10998),
 .UNSPECIFIED.,.F.,.F.,(4,2,2,2,2,2,4),(0.121154929624518,0.158718019202143,
0.238071711691698,0.317425404181253,0.396779096670807,0.476132789160362,
0.513695878737989),.UNSPECIFIED.);
#313=B_SPLINE_CURVE_WITH_KNOTS('',3,(#11023,#11024,#11025,#11026,#11027,
#11028,#11029,#11030,#11031,#11032,#11033,#11034,#11035,#11036),
 .UNSPECIFIED.,.F.,.F.,(4,2,2,2,2,2,4),(0.75600573798702,0.793568827564647,
0.872922520054201,0.952276212543756,1.03162990503331,1.11098359752287,1.14854668710049),
 .UNSPECIFIED.);
#314=B_SPLINE_CURVE_WITH_KNOTS('',3,(#11042,#11043,#11044,#11045,#11046,
#11047,#11048,#11049,#11050,#11051,#11052,#11053,#11054,#11055,#11056,#11057,
#11058,#11059),.UNSPECIFIED.,.F.,.F.,(4,2,2,2,2,2,2,2,4),(0.,0.0792028026112439,
0.158405605222488,0.237607602356377,0.316809599490267,0.396011596624156,
0.475213593758045,0.554416396369289,0.633619198980533),.UNSPECIFIED.);
#315=B_SPLINE_CURVE_WITH_KNOTS('',3,(#11060,#11061,#11062,#11063,#11064,
#11065,#11066,#11067,#11068,#11069,#11070,#11071,#11072,#11073,#11074,#11075,
#11076,#11077),.UNSPECIFIED.,.F.,.F.,(4,2,2,2,2,2,2,2,4),(0.633619198980533,
0.712822001591777,0.792024804203021,0.87122680133691,0.950428798470799,
1.02963079560469,1.10883279273858,1.18803559534982,1.26723839796107),
 .UNSPECIFIED.);
#316=B_SPLINE_CURVE_WITH_KNOTS('',3,(#11080,#11081,#11082,#11083,#11084,
#11085,#11086,#11087,#11088,#11089,#11090,#11091,#11092,#11093),
 .UNSPECIFIED.,.F.,.F.,(4,2,2,2,2,2,4),(0.121154929624516,0.158718019202143,
0.238071711691697,0.317425404181252,0.396779096670807,0.476132789160362,
0.513695878737989),.UNSPECIFIED.);
#317=B_SPLINE_CURVE_WITH_KNOTS('',3,(#11413,#11414,#11415,#11416,#11417,
#11418,#11419,#11420,#11421,#11422,#11423,#11424,#11425,#11426),
 .UNSPECIFIED.,.F.,.F.,(4,2,2,2,2,2,4),(0.75600573798702,0.793568827564648,
0.872922520054202,0.952276212543757,1.03162990503331,1.11098359752287,1.14854668710049),
 .UNSPECIFIED.);
#318=B_SPLINE_CURVE_WITH_KNOTS('',3,(#11434,#11435,#11436,#11437,#11438,
#11439,#11440,#11441,#11442,#11443,#11444,#11445,#11446,#11447),
 .UNSPECIFIED.,.F.,.F.,(4,2,2,2,2,2,4),(0.121154929624516,0.158718019202143,
0.238071711691698,0.317425404181252,0.396779096670807,0.476132789160362,
0.51369587873799),.UNSPECIFIED.);
#319=SPHERICAL_SURFACE('',#6928,2.35);
#320=SPHERICAL_SURFACE('',#6968,2.35);
#321=SHAPE_REPRESENTATION_RELATIONSHIP('SRR','None',#11947,#355);
#322=SHAPE_REPRESENTATION_RELATIONSHIP('SRR','None',#11948,#356);
#323=SHAPE_REPRESENTATION_RELATIONSHIP('SRR','None',#11949,#357);
#324=SHAPE_REPRESENTATION_RELATIONSHIP('SRR','None',#11950,#358);
#325=SHAPE_REPRESENTATION_RELATIONSHIP('SRR','None',#11951,#359);
#326=SHAPE_REPRESENTATION_RELATIONSHIP('SRR','None',#11952,#360);
#327=SHAPE_REPRESENTATION_RELATIONSHIP('SRR','None',#11953,#361);
#328=SHAPE_REPRESENTATION_RELATIONSHIP('SRR','None',#11954,#362);
#329=SHAPE_REPRESENTATION_RELATIONSHIP('SRR','None',#11955,#363);
#330=SHAPE_REPRESENTATION_RELATIONSHIP('SRR','None',#11956,#364);
#331=SHAPE_REPRESENTATION_RELATIONSHIP('SRR','None',#11957,#365);
#332=SHAPE_REPRESENTATION_RELATIONSHIP('SRR','None',#11958,#366);
#333=SHAPE_REPRESENTATION_RELATIONSHIP('SRR','None',#11959,#367);
#334=SHAPE_REPRESENTATION_RELATIONSHIP('SRR','None',#11960,#368);
#335=SHAPE_REPRESENTATION_RELATIONSHIP('SRR','None',#11961,#369);
#336=SHAPE_REPRESENTATION_RELATIONSHIP('SRR','None',#11963,#370);
#337=SHAPE_REPRESENTATION_RELATIONSHIP('SRR','None',#11964,#371);
#338=SHAPE_REPRESENTATION_RELATIONSHIP('SRR','None',#11965,#372);
#339=SHAPE_REPRESENTATION_RELATIONSHIP('SRR','None',#11966,#373);
#340=SHAPE_REPRESENTATION_RELATIONSHIP('SRR','None',#11967,#374);
#341=SHAPE_REPRESENTATION_RELATIONSHIP('SRR','None',#11969,#375);
#342=SHAPE_REPRESENTATION_RELATIONSHIP('SRR','None',#11970,#376);
#343=SHAPE_REPRESENTATION_RELATIONSHIP('SRR','None',#11971,#377);
#344=SHAPE_REPRESENTATION_RELATIONSHIP('SRR','None',#11972,#378);
#345=SHAPE_REPRESENTATION_RELATIONSHIP('SRR','None',#11973,#379);
#346=SHAPE_REPRESENTATION_RELATIONSHIP('SRR','None',#11974,#380);
#347=SHAPE_REPRESENTATION_RELATIONSHIP('SRR','None',#11975,#381);
#348=SHAPE_REPRESENTATION_RELATIONSHIP('SRR','None',#11976,#382);
#349=SHAPE_REPRESENTATION_RELATIONSHIP('SRR','None',#11977,#383);
#350=SHAPE_REPRESENTATION_RELATIONSHIP('SRR','None',#11978,#384);
#351=SHAPE_REPRESENTATION_RELATIONSHIP('SRR','None',#11979,#385);
#352=SHAPE_REPRESENTATION_RELATIONSHIP('SRR','None',#11980,#386);
#353=SHAPE_REPRESENTATION_RELATIONSHIP('SRR','None',#11981,#387);
#354=SHAPE_REPRESENTATION_RELATIONSHIP('SRR','None',#11983,#388);
#355=ADVANCED_BREP_SHAPE_REPRESENTATION('',(#424),#11764);
#356=ADVANCED_BREP_SHAPE_REPRESENTATION('',(#425),#11765);
#357=ADVANCED_BREP_SHAPE_REPRESENTATION('',(#426),#11766);
#358=ADVANCED_BREP_SHAPE_REPRESENTATION('',(#427),#11767);
#359=ADVANCED_BREP_SHAPE_REPRESENTATION('',(#428),#11768);
#360=ADVANCED_BREP_SHAPE_REPRESENTATION('',(#429),#11769);
#361=ADVANCED_BREP_SHAPE_REPRESENTATION('',(#430),#11770);
#362=ADVANCED_BREP_SHAPE_REPRESENTATION('',(#431),#11771);
#363=ADVANCED_BREP_SHAPE_REPRESENTATION('',(#432),#11772);
#364=ADVANCED_BREP_SHAPE_REPRESENTATION('',(#433),#11773);
#365=ADVANCED_BREP_SHAPE_REPRESENTATION('',(#434),#11774);
#366=ADVANCED_BREP_SHAPE_REPRESENTATION('',(#435),#11775);
#367=ADVANCED_BREP_SHAPE_REPRESENTATION('',(#436),#11776);
#368=ADVANCED_BREP_SHAPE_REPRESENTATION('',(#437),#11777);
#369=ADVANCED_BREP_SHAPE_REPRESENTATION('',(#438),#11778);
#370=ADVANCED_BREP_SHAPE_REPRESENTATION('',(#439),#11780);
#371=ADVANCED_BREP_SHAPE_REPRESENTATION('',(#440,#441),#11781);
#372=ADVANCED_BREP_SHAPE_REPRESENTATION('',(#442),#11782);
#373=ADVANCED_BREP_SHAPE_REPRESENTATION('',(#26),#11783);
#374=ADVANCED_BREP_SHAPE_REPRESENTATION('',(#27),#11784);
#375=ADVANCED_BREP_SHAPE_REPRESENTATION('',(#443),#11786);
#376=ADVANCED_BREP_SHAPE_REPRESENTATION('',(#444),#11787);
#377=ADVANCED_BREP_SHAPE_REPRESENTATION('',(#445),#11788);
#378=ADVANCED_BREP_SHAPE_REPRESENTATION('',(#446),#11789);
#379=ADVANCED_BREP_SHAPE_REPRESENTATION('',(#447),#11790);
#380=ADVANCED_BREP_SHAPE_REPRESENTATION('',(#448),#11791);
#381=ADVANCED_BREP_SHAPE_REPRESENTATION('',(#449),#11792);
#382=ADVANCED_BREP_SHAPE_REPRESENTATION('',(#450),#11793);
#383=ADVANCED_BREP_SHAPE_REPRESENTATION('',(#451),#11794);
#384=ADVANCED_BREP_SHAPE_REPRESENTATION('',(#452),#11795);
#385=ADVANCED_BREP_SHAPE_REPRESENTATION('',(#453),#11796);
#386=ADVANCED_BREP_SHAPE_REPRESENTATION('',(#454),#11797);
#387=ADVANCED_BREP_SHAPE_REPRESENTATION('',(#28),#11798);
#388=ADVANCED_BREP_SHAPE_REPRESENTATION('',(#455),#11800);
#389=STYLED_ITEM('',(#12192),#424);
#390=STYLED_ITEM('',(#12227),#425);
#391=STYLED_ITEM('',(#12227),#426);
#392=STYLED_ITEM('',(#12213),#427);
#393=STYLED_ITEM('',(#12206),#428);
#394=STYLED_ITEM('',(#12206),#429);
#395=STYLED_ITEM('',(#12213),#430);
#396=STYLED_ITEM('',(#12206),#431);
#397=STYLED_ITEM('',(#12206),#432);
#398=STYLED_ITEM('',(#12206),#433);
#399=STYLED_ITEM('',(#12213),#434);
#400=STYLED_ITEM('',(#12227),#435);
#401=STYLED_ITEM('',(#12213),#436);
#402=STYLED_ITEM('',(#12213),#437);
#403=STYLED_ITEM('',(#12213),#438);
#404=STYLED_ITEM('',(#12192),#439);
#405=STYLED_ITEM('',(#12213),#440);
#406=STYLED_ITEM('',(#12213),#441);
#407=STYLED_ITEM('',(#12220),#442);
#408=STYLED_ITEM('',(#12220),#26);
#409=STYLED_ITEM('',(#12220),#27);
#410=STYLED_ITEM('',(#12213),#443);
#411=STYLED_ITEM('',(#12213),#444);
#412=STYLED_ITEM('',(#12213),#445);
#413=STYLED_ITEM('',(#12227),#446);
#414=STYLED_ITEM('',(#12199),#447);
#415=STYLED_ITEM('',(#12199),#448);
#416=STYLED_ITEM('',(#12199),#449);
#417=STYLED_ITEM('',(#12199),#450);
#418=STYLED_ITEM('',(#12206),#451);
#419=STYLED_ITEM('',(#12227),#452);
#420=STYLED_ITEM('',(#12206),#453);
#421=STYLED_ITEM('',(#12220),#454);
#422=STYLED_ITEM('',(#12220),#28);
#423=STYLED_ITEM('',(#12199),#455);
#424=MANIFOLD_SOLID_BREP('Body1',#6266);
#425=MANIFOLD_SOLID_BREP('Body1',#6267);
#426=MANIFOLD_SOLID_BREP('Body1',#6268);
#427=MANIFOLD_SOLID_BREP('Body1',#6269);
#428=MANIFOLD_SOLID_BREP('Body1',#6270);
#429=MANIFOLD_SOLID_BREP('Body1',#6271);
#430=MANIFOLD_SOLID_BREP('Body1',#6272);
#431=MANIFOLD_SOLID_BREP('Body1',#6273);
#432=MANIFOLD_SOLID_BREP('Body1',#6274);
#433=MANIFOLD_SOLID_BREP('Body1',#6275);
#434=MANIFOLD_SOLID_BREP('Body1',#6276);
#435=MANIFOLD_SOLID_BREP('Body1',#6277);
#436=MANIFOLD_SOLID_BREP('Body1',#6278);
#437=MANIFOLD_SOLID_BREP('Body1',#6279);
#438=MANIFOLD_SOLID_BREP('Body1',#6280);
#439=MANIFOLD_SOLID_BREP('Body1',#6281);
#440=MANIFOLD_SOLID_BREP('Body1',#6282);
#441=MANIFOLD_SOLID_BREP('Body2',#6283);
#442=MANIFOLD_SOLID_BREP('Body1',#6284);
#443=MANIFOLD_SOLID_BREP('Body1',#6289);
#444=MANIFOLD_SOLID_BREP('Body1',#6290);
#445=MANIFOLD_SOLID_BREP('Body1',#6291);
#446=MANIFOLD_SOLID_BREP('Body1',#6292);
#447=MANIFOLD_SOLID_BREP('Body1',#6293);
#448=MANIFOLD_SOLID_BREP('Body1',#6294);
#449=MANIFOLD_SOLID_BREP('Body1',#6295);
#450=MANIFOLD_SOLID_BREP('Body1',#6296);
#451=MANIFOLD_SOLID_BREP('Body1',#6297);
#452=MANIFOLD_SOLID_BREP('Body1',#6298);
#453=MANIFOLD_SOLID_BREP('Body1',#6299);
#454=MANIFOLD_SOLID_BREP('Body1',#6300);
#455=MANIFOLD_SOLID_BREP('Body1',#6303);
#456=FACE_BOUND('',#1211,.T.);
#457=FACE_BOUND('',#1212,.T.);
#458=FACE_BOUND('',#1213,.T.);
#459=FACE_BOUND('',#1214,.T.);
#460=FACE_BOUND('',#1215,.T.);
#461=FACE_BOUND('',#1216,.T.);
#462=FACE_BOUND('',#1217,.T.);
#463=FACE_BOUND('',#1218,.T.);
#464=FACE_BOUND('',#1219,.T.);
#465=FACE_BOUND('',#1220,.T.);
#466=FACE_BOUND('',#1222,.T.);
#467=FACE_BOUND('',#1223,.T.);
#468=FACE_BOUND('',#1224,.T.);
#469=FACE_BOUND('',#1225,.T.);
#470=FACE_BOUND('',#1226,.T.);
#471=FACE_BOUND('',#1227,.T.);
#472=FACE_BOUND('',#1228,.T.);
#473=FACE_BOUND('',#1229,.T.);
#474=FACE_BOUND('',#1230,.T.);
#475=FACE_BOUND('',#1231,.T.);
#476=FACE_BOUND('',#1246,.T.);
#477=FACE_BOUND('',#1249,.T.);
#478=FACE_BOUND('',#1254,.T.);
#479=FACE_BOUND('',#1257,.T.);
#480=FACE_BOUND('',#1267,.T.);
#481=FACE_BOUND('',#1268,.T.);
#482=FACE_BOUND('',#1269,.T.);
#483=FACE_BOUND('',#1270,.T.);
#484=FACE_BOUND('',#1271,.T.);
#485=FACE_BOUND('',#1272,.T.);
#486=FACE_BOUND('',#1274,.T.);
#487=FACE_BOUND('',#1275,.T.);
#488=FACE_BOUND('',#1276,.T.);
#489=FACE_BOUND('',#1277,.T.);
#490=FACE_BOUND('',#1278,.T.);
#491=FACE_BOUND('',#1279,.T.);
#492=FACE_BOUND('',#1283,.T.);
#493=FACE_BOUND('',#1285,.T.);
#494=FACE_BOUND('',#1289,.T.);
#495=FACE_BOUND('',#1291,.T.);
#496=FACE_BOUND('',#1294,.T.);
#497=FACE_BOUND('',#1297,.T.);
#498=FACE_BOUND('',#1302,.T.);
#499=FACE_BOUND('',#1305,.T.);
#500=FACE_BOUND('',#1315,.T.);
#501=FACE_BOUND('',#1316,.T.);
#502=FACE_BOUND('',#1317,.T.);
#503=FACE_BOUND('',#1318,.T.);
#504=FACE_BOUND('',#1319,.T.);
#505=FACE_BOUND('',#1320,.T.);
#506=FACE_BOUND('',#1322,.T.);
#507=FACE_BOUND('',#1323,.T.);
#508=FACE_BOUND('',#1324,.T.);
#509=FACE_BOUND('',#1325,.T.);
#510=FACE_BOUND('',#1326,.T.);
#511=FACE_BOUND('',#1327,.T.);
#512=FACE_BOUND('',#1331,.T.);
#513=FACE_BOUND('',#1333,.T.);
#514=FACE_BOUND('',#1337,.T.);
#515=FACE_BOUND('',#1339,.T.);
#516=FACE_BOUND('',#1344,.T.);
#517=FACE_BOUND('',#1345,.T.);
#518=FACE_BOUND('',#1346,.T.);
#519=FACE_BOUND('',#1352,.T.);
#520=FACE_BOUND('',#1355,.T.);
#521=FACE_BOUND('',#1359,.T.);
#522=FACE_BOUND('',#1360,.T.);
#523=FACE_BOUND('',#1364,.T.);
#524=FACE_BOUND('',#1369,.T.);
#525=FACE_BOUND('',#1373,.T.);
#526=FACE_BOUND('',#1375,.T.);
#527=FACE_BOUND('',#1379,.T.);
#528=FACE_BOUND('',#1381,.T.);
#529=FACE_BOUND('',#1394,.T.);
#530=FACE_BOUND('',#1396,.T.);
#531=FACE_BOUND('',#1400,.T.);
#532=FACE_BOUND('',#1401,.T.);
#533=FACE_BOUND('',#1409,.T.);
#534=FACE_BOUND('',#1410,.T.);
#535=FACE_BOUND('',#1411,.T.);
#536=FACE_BOUND('',#1414,.T.);
#537=FACE_BOUND('',#1416,.T.);
#538=FACE_BOUND('',#1429,.T.);
#539=FACE_BOUND('',#1430,.T.);
#540=FACE_BOUND('',#1431,.T.);
#541=FACE_BOUND('',#1434,.T.);
#542=FACE_BOUND('',#1436,.T.);
#543=FACE_BOUND('',#1437,.T.);
#544=FACE_BOUND('',#1439,.T.);
#545=FACE_BOUND('',#1443,.T.);
#546=FACE_BOUND('',#1444,.T.);
#547=FACE_BOUND('',#1445,.T.);
#548=FACE_BOUND('',#1446,.T.);
#549=FACE_BOUND('',#1447,.T.);
#550=FACE_BOUND('',#1448,.T.);
#551=FACE_BOUND('',#1454,.T.);
#552=FACE_BOUND('',#1456,.T.);
#553=FACE_BOUND('',#1459,.T.);
#554=FACE_BOUND('',#1461,.T.);
#555=FACE_BOUND('',#1462,.T.);
#556=FACE_BOUND('',#1463,.T.);
#557=FACE_BOUND('',#1464,.T.);
#558=FACE_BOUND('',#1465,.T.);
#559=FACE_BOUND('',#1466,.T.);
#560=FACE_BOUND('',#1470,.T.);
#561=FACE_BOUND('',#1472,.T.);
#562=FACE_BOUND('',#1487,.T.);
#563=FACE_BOUND('',#1504,.T.);
#564=FACE_BOUND('',#1514,.T.);
#565=FACE_BOUND('',#1516,.T.);
#566=FACE_BOUND('',#1518,.T.);
#567=FACE_BOUND('',#1520,.T.);
#568=FACE_BOUND('',#1525,.T.);
#569=FACE_BOUND('',#1527,.T.);
#570=FACE_BOUND('',#1529,.T.);
#571=FACE_BOUND('',#1531,.T.);
#572=FACE_BOUND('',#1535,.T.);
#573=FACE_BOUND('',#1537,.T.);
#574=FACE_BOUND('',#1541,.T.);
#575=FACE_BOUND('',#1543,.T.);
#576=FACE_BOUND('',#1548,.T.);
#577=FACE_BOUND('',#1550,.T.);
#578=FACE_BOUND('',#1552,.T.);
#579=FACE_BOUND('',#1554,.T.);
#580=FACE_BOUND('',#1558,.T.);
#581=FACE_BOUND('',#1560,.T.);
#582=FACE_BOUND('',#1565,.T.);
#583=FACE_BOUND('',#1567,.T.);
#584=FACE_BOUND('',#1569,.T.);
#585=FACE_BOUND('',#1571,.T.);
#586=FACE_BOUND('',#1576,.T.);
#587=FACE_BOUND('',#1578,.T.);
#588=FACE_BOUND('',#1580,.T.);
#589=FACE_BOUND('',#1630,.T.);
#590=FACE_BOUND('',#1632,.T.);
#591=FACE_BOUND('',#1639,.T.);
#592=FACE_BOUND('',#1640,.T.);
#593=FACE_BOUND('',#1643,.T.);
#594=FACE_BOUND('',#1648,.T.);
#595=FACE_BOUND('',#1650,.T.);
#596=FACE_BOUND('',#1655,.T.);
#597=FACE_BOUND('',#1665,.T.);
#598=FACE_BOUND('',#1675,.T.);
#599=FACE_BOUND('',#1692,.T.);
#600=FACE_BOUND('',#1696,.T.);
#601=PLANE('',#6712);
#602=PLANE('',#6713);
#603=PLANE('',#6714);
#604=PLANE('',#6715);
#605=PLANE('',#6716);
#606=PLANE('',#6717);
#607=PLANE('',#6719);
#608=PLANE('',#6720);
#609=PLANE('',#6721);
#610=PLANE('',#6722);
#611=PLANE('',#6723);
#612=PLANE('',#6724);
#613=PLANE('',#6726);
#614=PLANE('',#6727);
#615=PLANE('',#6728);
#616=PLANE('',#6729);
#617=PLANE('',#6730);
#618=PLANE('',#6731);
#619=PLANE('',#6736);
#620=PLANE('',#6741);
#621=PLANE('',#6750);
#622=PLANE('',#6755);
#623=PLANE('',#6767);
#624=PLANE('',#6768);
#625=PLANE('',#6769);
#626=PLANE('',#6770);
#627=PLANE('',#6771);
#628=PLANE('',#6772);
#629=PLANE('',#6780);
#630=PLANE('',#6781);
#631=PLANE('',#6789);
#632=PLANE('',#6790);
#633=PLANE('',#6795);
#634=PLANE('',#6800);
#635=PLANE('',#6809);
#636=PLANE('',#6814);
#637=PLANE('',#6826);
#638=PLANE('',#6827);
#639=PLANE('',#6828);
#640=PLANE('',#6829);
#641=PLANE('',#6830);
#642=PLANE('',#6831);
#643=PLANE('',#6839);
#644=PLANE('',#6840);
#645=PLANE('',#6848);
#646=PLANE('',#6849);
#647=PLANE('',#6860);
#648=PLANE('',#6861);
#649=PLANE('',#6862);
#650=PLANE('',#6863);
#651=PLANE('',#6864);
#652=PLANE('',#6865);
#653=PLANE('',#6866);
#654=PLANE('',#6867);
#655=PLANE('',#6868);
#656=PLANE('',#6869);
#657=PLANE('',#6870);
#658=PLANE('',#6875);
#659=PLANE('',#6876);
#660=PLANE('',#6881);
#661=PLANE('',#6884);
#662=PLANE('',#6892);
#663=PLANE('',#6893);
#664=PLANE('',#6901);
#665=PLANE('',#6902);
#666=PLANE('',#6904);
#667=PLANE('',#6905);
#668=PLANE('',#6906);
#669=PLANE('',#6907);
#670=PLANE('',#6908);
#671=PLANE('',#6909);
#672=PLANE('',#6914);
#673=PLANE('',#6915);
#674=PLANE('',#6916);
#675=PLANE('',#6917);
#676=PLANE('',#6918);
#677=PLANE('',#6919);
#678=PLANE('',#6930);
#679=PLANE('',#6932);
#680=PLANE('',#6934);
#681=PLANE('',#6936);
#682=PLANE('',#6937);
#683=PLANE('',#6939);
#684=PLANE('',#6940);
#685=PLANE('',#6946);
#686=PLANE('',#6947);
#687=PLANE('',#6948);
#688=PLANE('',#6949);
#689=PLANE('',#6950);
#690=PLANE('',#6951);
#691=PLANE('',#6952);
#692=PLANE('',#6957);
#693=PLANE('',#6958);
#694=PLANE('',#6959);
#695=PLANE('',#6960);
#696=PLANE('',#6961);
#697=PLANE('',#6966);
#698=PLANE('',#6971);
#699=PLANE('',#6981);
#700=PLANE('',#6983);
#701=PLANE('',#6987);
#702=PLANE('',#6999);
#703=PLANE('',#7000);
#704=PLANE('',#7002);
#705=PLANE('',#7003);
#706=PLANE('',#7004);
#707=PLANE('',#7005);
#708=PLANE('',#7006);
#709=PLANE('',#7007);
#710=PLANE('',#7008);
#711=PLANE('',#7009);
#712=PLANE('',#7010);
#713=PLANE('',#7012);
#714=PLANE('',#7020);
#715=PLANE('',#7026);
#716=PLANE('',#7027);
#717=PLANE('',#7028);
#718=PLANE('',#7029);
#719=PLANE('',#7030);
#720=PLANE('',#7031);
#721=PLANE('',#7032);
#722=PLANE('',#7033);
#723=PLANE('',#7034);
#724=PLANE('',#7036);
#725=PLANE('',#7044);
#726=PLANE('',#7054);
#727=PLANE('',#7055);
#728=PLANE('',#7057);
#729=PLANE('',#7062);
#730=PLANE('',#7069);
#731=PLANE('',#7070);
#732=PLANE('',#7072);
#733=PLANE('',#7077);
#734=PLANE('',#7084);
#735=PLANE('',#7085);
#736=PLANE('',#7093);
#737=PLANE('',#7094);
#738=PLANE('',#7102);
#739=PLANE('',#7103);
#740=PLANE('',#7105);
#741=PLANE('',#7110);
#742=PLANE('',#7117);
#743=PLANE('',#7118);
#744=PLANE('',#7126);
#745=PLANE('',#7127);
#746=PLANE('',#7129);
#747=PLANE('',#7134);
#748=PLANE('',#7141);
#749=PLANE('',#7142);
#750=PLANE('',#7144);
#751=PLANE('',#7149);
#752=PLANE('',#7153);
#753=PLANE('',#7157);
#754=PLANE('',#7158);
#755=PLANE('',#7159);
#756=PLANE('',#7160);
#757=PLANE('',#7161);
#758=PLANE('',#7162);
#759=PLANE('',#7163);
#760=PLANE('',#7164);
#761=PLANE('',#7165);
#762=PLANE('',#7166);
#763=PLANE('',#7167);
#764=PLANE('',#7168);
#765=PLANE('',#7169);
#766=PLANE('',#7170);
#767=PLANE('',#7171);
#768=PLANE('',#7172);
#769=PLANE('',#7173);
#770=PLANE('',#7174);
#771=PLANE('',#7175);
#772=PLANE('',#7176);
#773=PLANE('',#7177);
#774=PLANE('',#7178);
#775=PLANE('',#7179);
#776=PLANE('',#7180);
#777=PLANE('',#7181);
#778=PLANE('',#7182);
#779=PLANE('',#7183);
#780=PLANE('',#7184);
#781=PLANE('',#7185);
#782=PLANE('',#7186);
#783=PLANE('',#7187);
#784=PLANE('',#7188);
#785=PLANE('',#7189);
#786=PLANE('',#7190);
#787=PLANE('',#7191);
#788=PLANE('',#7192);
#789=PLANE('',#7193);
#790=PLANE('',#7194);
#791=PLANE('',#7195);
#792=PLANE('',#7196);
#793=PLANE('',#7197);
#794=PLANE('',#7198);
#795=PLANE('',#7199);
#796=PLANE('',#7200);
#797=PLANE('',#7201);
#798=PLANE('',#7202);
#799=PLANE('',#7203);
#800=PLANE('',#7204);
#801=PLANE('',#7205);
#802=PLANE('',#7206);
#803=PLANE('',#7211);
#804=PLANE('',#7217);
#805=PLANE('',#7218);
#806=PLANE('',#7219);
#807=PLANE('',#7223);
#808=PLANE('',#7224);
#809=PLANE('',#7226);
#810=PLANE('',#7227);
#811=PLANE('',#7232);
#812=PLANE('',#7237);
#813=PLANE('',#7241);
#814=PLANE('',#7242);
#815=PLANE('',#7244);
#816=PLANE('',#7245);
#817=PLANE('',#7246);
#818=PLANE('',#7247);
#819=PLANE('',#7248);
#820=PLANE('',#7249);
#821=PLANE('',#7250);
#822=PLANE('',#7251);
#823=PLANE('',#7259);
#824=PLANE('',#7261);
#825=PLANE('',#7269);
#826=PLANE('',#7277);
#827=PLANE('',#7278);
#828=PLANE('',#7279);
#829=PLANE('',#7280);
#830=PLANE('',#7281);
#831=PLANE('',#7282);
#832=PLANE('',#7283);
#833=PLANE('',#7284);
#834=PLANE('',#7285);
#835=PLANE('',#7349);
#836=PLANE('',#7350);
#837=PLANE('',#7351);
#838=PLANE('',#7352);
#839=PLANE('',#7353);
#840=FACE_OUTER_BOUND('',#1196,.T.);
#841=FACE_OUTER_BOUND('',#1197,.T.);
#842=FACE_OUTER_BOUND('',#1198,.T.);
#843=FACE_OUTER_BOUND('',#1199,.T.);
#844=FACE_OUTER_BOUND('',#1200,.T.);
#845=FACE_OUTER_BOUND('',#1201,.T.);
#846=FACE_OUTER_BOUND('',#1202,.T.);
#847=FACE_OUTER_BOUND('',#1203,.T.);
#848=FACE_OUTER_BOUND('',#1204,.T.);
#849=FACE_OUTER_BOUND('',#1205,.T.);
#850=FACE_OUTER_BOUND('',#1206,.T.);
#851=FACE_OUTER_BOUND('',#1207,.T.);
#852=FACE_OUTER_BOUND('',#1208,.T.);
#853=FACE_OUTER_BOUND('',#1209,.T.);
#854=FACE_OUTER_BOUND('',#1210,.T.);
#855=FACE_OUTER_BOUND('',#1221,.T.);
#856=FACE_OUTER_BOUND('',#1232,.T.);
#857=FACE_OUTER_BOUND('',#1233,.T.);
#858=FACE_OUTER_BOUND('',#1234,.T.);
#859=FACE_OUTER_BOUND('',#1235,.T.);
#860=FACE_OUTER_BOUND('',#1236,.T.);
#861=FACE_OUTER_BOUND('',#1237,.T.);
#862=FACE_OUTER_BOUND('',#1238,.T.);
#863=FACE_OUTER_BOUND('',#1239,.T.);
#864=FACE_OUTER_BOUND('',#1240,.T.);
#865=FACE_OUTER_BOUND('',#1241,.T.);
#866=FACE_OUTER_BOUND('',#1242,.T.);
#867=FACE_OUTER_BOUND('',#1243,.T.);
#868=FACE_OUTER_BOUND('',#1244,.T.);
#869=FACE_OUTER_BOUND('',#1245,.T.);
#870=FACE_OUTER_BOUND('',#1247,.T.);
#871=FACE_OUTER_BOUND('',#1248,.T.);
#872=FACE_OUTER_BOUND('',#1250,.T.);
#873=FACE_OUTER_BOUND('',#1251,.T.);
#874=FACE_OUTER_BOUND('',#1252,.T.);
#875=FACE_OUTER_BOUND('',#1253,.T.);
#876=FACE_OUTER_BOUND('',#1255,.T.);
#877=FACE_OUTER_BOUND('',#1256,.T.);
#878=FACE_OUTER_BOUND('',#1258,.T.);
#879=FACE_OUTER_BOUND('',#1259,.T.);
#880=FACE_OUTER_BOUND('',#1260,.T.);
#881=FACE_OUTER_BOUND('',#1261,.T.);
#882=FACE_OUTER_BOUND('',#1262,.T.);
#883=FACE_OUTER_BOUND('',#1263,.T.);
#884=FACE_OUTER_BOUND('',#1264,.T.);
#885=FACE_OUTER_BOUND('',#1265,.T.);
#886=FACE_OUTER_BOUND('',#1266,.T.);
#887=FACE_OUTER_BOUND('',#1273,.T.);
#888=FACE_OUTER_BOUND('',#1280,.T.);
#889=FACE_OUTER_BOUND('',#1281,.T.);
#890=FACE_OUTER_BOUND('',#1282,.T.);
#891=FACE_OUTER_BOUND('',#1284,.T.);
#892=FACE_OUTER_BOUND('',#1286,.T.);
#893=FACE_OUTER_BOUND('',#1287,.T.);
#894=FACE_OUTER_BOUND('',#1288,.T.);
#895=FACE_OUTER_BOUND('',#1290,.T.);
#896=FACE_OUTER_BOUND('',#1292,.T.);
#897=FACE_OUTER_BOUND('',#1293,.T.);
#898=FACE_OUTER_BOUND('',#1295,.T.);
#899=FACE_OUTER_BOUND('',#1296,.T.);
#900=FACE_OUTER_BOUND('',#1298,.T.);
#901=FACE_OUTER_BOUND('',#1299,.T.);
#902=FACE_OUTER_BOUND('',#1300,.T.);
#903=FACE_OUTER_BOUND('',#1301,.T.);
#904=FACE_OUTER_BOUND('',#1303,.T.);
#905=FACE_OUTER_BOUND('',#1304,.T.);
#906=FACE_OUTER_BOUND('',#1306,.T.);
#907=FACE_OUTER_BOUND('',#1307,.T.);
#908=FACE_OUTER_BOUND('',#1308,.T.);
#909=FACE_OUTER_BOUND('',#1309,.T.);
#910=FACE_OUTER_BOUND('',#1310,.T.);
#911=FACE_OUTER_BOUND('',#1311,.T.);
#912=FACE_OUTER_BOUND('',#1312,.T.);
#913=FACE_OUTER_BOUND('',#1313,.T.);
#914=FACE_OUTER_BOUND('',#1314,.T.);
#915=FACE_OUTER_BOUND('',#1321,.T.);
#916=FACE_OUTER_BOUND('',#1328,.T.);
#917=FACE_OUTER_BOUND('',#1329,.T.);
#918=FACE_OUTER_BOUND('',#1330,.T.);
#919=FACE_OUTER_BOUND('',#1332,.T.);
#920=FACE_OUTER_BOUND('',#1334,.T.);
#921=FACE_OUTER_BOUND('',#1335,.T.);
#922=FACE_OUTER_BOUND('',#1336,.T.);
#923=FACE_OUTER_BOUND('',#1338,.T.);
#924=FACE_OUTER_BOUND('',#1340,.T.);
#925=FACE_OUTER_BOUND('',#1341,.T.);
#926=FACE_OUTER_BOUND('',#1342,.T.);
#927=FACE_OUTER_BOUND('',#1343,.T.);
#928=FACE_OUTER_BOUND('',#1347,.T.);
#929=FACE_OUTER_BOUND('',#1348,.T.);
#930=FACE_OUTER_BOUND('',#1349,.T.);
#931=FACE_OUTER_BOUND('',#1350,.T.);
#932=FACE_OUTER_BOUND('',#1351,.T.);
#933=FACE_OUTER_BOUND('',#1353,.T.);
#934=FACE_OUTER_BOUND('',#1354,.T.);
#935=FACE_OUTER_BOUND('',#1356,.T.);
#936=FACE_OUTER_BOUND('',#1357,.T.);
#937=FACE_OUTER_BOUND('',#1358,.T.);
#938=FACE_OUTER_BOUND('',#1361,.T.);
#939=FACE_OUTER_BOUND('',#1362,.T.);
#940=FACE_OUTER_BOUND('',#1363,.T.);
#941=FACE_OUTER_BOUND('',#1365,.T.);
#942=FACE_OUTER_BOUND('',#1366,.T.);
#943=FACE_OUTER_BOUND('',#1367,.T.);
#944=FACE_OUTER_BOUND('',#1368,.T.);
#945=FACE_OUTER_BOUND('',#1370,.T.);
#946=FACE_OUTER_BOUND('',#1371,.T.);
#947=FACE_OUTER_BOUND('',#1372,.T.);
#948=FACE_OUTER_BOUND('',#1374,.T.);
#949=FACE_OUTER_BOUND('',#1376,.T.);
#950=FACE_OUTER_BOUND('',#1377,.T.);
#951=FACE_OUTER_BOUND('',#1378,.T.);
#952=FACE_OUTER_BOUND('',#1380,.T.);
#953=FACE_OUTER_BOUND('',#1382,.T.);
#954=FACE_OUTER_BOUND('',#1383,.T.);
#955=FACE_OUTER_BOUND('',#1384,.T.);
#956=FACE_OUTER_BOUND('',#1385,.T.);
#957=FACE_OUTER_BOUND('',#1386,.T.);
#958=FACE_OUTER_BOUND('',#1387,.T.);
#959=FACE_OUTER_BOUND('',#1388,.T.);
#960=FACE_OUTER_BOUND('',#1389,.T.);
#961=FACE_OUTER_BOUND('',#1390,.T.);
#962=FACE_OUTER_BOUND('',#1391,.T.);
#963=FACE_OUTER_BOUND('',#1392,.T.);
#964=FACE_OUTER_BOUND('',#1393,.T.);
#965=FACE_OUTER_BOUND('',#1395,.T.);
#966=FACE_OUTER_BOUND('',#1397,.T.);
#967=FACE_OUTER_BOUND('',#1398,.T.);
#968=FACE_OUTER_BOUND('',#1399,.T.);
#969=FACE_OUTER_BOUND('',#1402,.T.);
#970=FACE_OUTER_BOUND('',#1403,.T.);
#971=FACE_OUTER_BOUND('',#1404,.T.);
#972=FACE_OUTER_BOUND('',#1405,.T.);
#973=FACE_OUTER_BOUND('',#1406,.T.);
#974=FACE_OUTER_BOUND('',#1407,.T.);
#975=FACE_OUTER_BOUND('',#1408,.T.);
#976=FACE_OUTER_BOUND('',#1412,.T.);
#977=FACE_OUTER_BOUND('',#1413,.T.);
#978=FACE_OUTER_BOUND('',#1415,.T.);
#979=FACE_OUTER_BOUND('',#1417,.T.);
#980=FACE_OUTER_BOUND('',#1418,.T.);
#981=FACE_OUTER_BOUND('',#1419,.T.);
#982=FACE_OUTER_BOUND('',#1420,.T.);
#983=FACE_OUTER_BOUND('',#1421,.T.);
#984=FACE_OUTER_BOUND('',#1422,.T.);
#985=FACE_OUTER_BOUND('',#1423,.T.);
#986=FACE_OUTER_BOUND('',#1424,.T.);
#987=FACE_OUTER_BOUND('',#1425,.T.);
#988=FACE_OUTER_BOUND('',#1426,.T.);
#989=FACE_OUTER_BOUND('',#1427,.T.);
#990=FACE_OUTER_BOUND('',#1428,.T.);
#991=FACE_OUTER_BOUND('',#1432,.T.);
#992=FACE_OUTER_BOUND('',#1433,.T.);
#993=FACE_OUTER_BOUND('',#1435,.T.);
#994=FACE_OUTER_BOUND('',#1438,.T.);
#995=FACE_OUTER_BOUND('',#1440,.T.);
#996=FACE_OUTER_BOUND('',#1441,.T.);
#997=FACE_OUTER_BOUND('',#1442,.T.);
#998=FACE_OUTER_BOUND('',#1449,.T.);
#999=FACE_OUTER_BOUND('',#1450,.T.);
#1000=FACE_OUTER_BOUND('',#1451,.T.);
#1001=FACE_OUTER_BOUND('',#1452,.T.);
#1002=FACE_OUTER_BOUND('',#1453,.T.);
#1003=FACE_OUTER_BOUND('',#1455,.T.);
#1004=FACE_OUTER_BOUND('',#1457,.T.);
#1005=FACE_OUTER_BOUND('',#1458,.T.);
#1006=FACE_OUTER_BOUND('',#1460,.T.);
#1007=FACE_OUTER_BOUND('',#1467,.T.);
#1008=FACE_OUTER_BOUND('',#1468,.T.);
#1009=FACE_OUTER_BOUND('',#1469,.T.);
#1010=FACE_OUTER_BOUND('',#1471,.T.);
#1011=FACE_OUTER_BOUND('',#1473,.T.);
#1012=FACE_OUTER_BOUND('',#1474,.T.);
#1013=FACE_OUTER_BOUND('',#1475,.T.);
#1014=FACE_OUTER_BOUND('',#1476,.T.);
#1015=FACE_OUTER_BOUND('',#1477,.T.);
#1016=FACE_OUTER_BOUND('',#1478,.T.);
#1017=FACE_OUTER_BOUND('',#1479,.T.);
#1018=FACE_OUTER_BOUND('',#1480,.T.);
#1019=FACE_OUTER_BOUND('',#1481,.T.);
#1020=FACE_OUTER_BOUND('',#1482,.T.);
#1021=FACE_OUTER_BOUND('',#1483,.T.);
#1022=FACE_OUTER_BOUND('',#1484,.T.);
#1023=FACE_OUTER_BOUND('',#1485,.T.);
#1024=FACE_OUTER_BOUND('',#1486,.T.);
#1025=FACE_OUTER_BOUND('',#1488,.T.);
#1026=FACE_OUTER_BOUND('',#1489,.T.);
#1027=FACE_OUTER_BOUND('',#1490,.T.);
#1028=FACE_OUTER_BOUND('',#1491,.T.);
#1029=FACE_OUTER_BOUND('',#1492,.T.);
#1030=FACE_OUTER_BOUND('',#1493,.T.);
#1031=FACE_OUTER_BOUND('',#1494,.T.);
#1032=FACE_OUTER_BOUND('',#1495,.T.);
#1033=FACE_OUTER_BOUND('',#1496,.T.);
#1034=FACE_OUTER_BOUND('',#1497,.T.);
#1035=FACE_OUTER_BOUND('',#1498,.T.);
#1036=FACE_OUTER_BOUND('',#1499,.T.);
#1037=FACE_OUTER_BOUND('',#1500,.T.);
#1038=FACE_OUTER_BOUND('',#1501,.T.);
#1039=FACE_OUTER_BOUND('',#1502,.T.);
#1040=FACE_OUTER_BOUND('',#1503,.T.);
#1041=FACE_OUTER_BOUND('',#1505,.T.);
#1042=FACE_OUTER_BOUND('',#1506,.T.);
#1043=FACE_OUTER_BOUND('',#1507,.T.);
#1044=FACE_OUTER_BOUND('',#1508,.T.);
#1045=FACE_OUTER_BOUND('',#1509,.T.);
#1046=FACE_OUTER_BOUND('',#1510,.T.);
#1047=FACE_OUTER_BOUND('',#1511,.T.);
#1048=FACE_OUTER_BOUND('',#1512,.T.);
#1049=FACE_OUTER_BOUND('',#1513,.T.);
#1050=FACE_OUTER_BOUND('',#1515,.T.);
#1051=FACE_OUTER_BOUND('',#1517,.T.);
#1052=FACE_OUTER_BOUND('',#1519,.T.);
#1053=FACE_OUTER_BOUND('',#1521,.T.);
#1054=FACE_OUTER_BOUND('',#1522,.T.);
#1055=FACE_OUTER_BOUND('',#1523,.T.);
#1056=FACE_OUTER_BOUND('',#1524,.T.);
#1057=FACE_OUTER_BOUND('',#1526,.T.);
#1058=FACE_OUTER_BOUND('',#1528,.T.);
#1059=FACE_OUTER_BOUND('',#1530,.T.);
#1060=FACE_OUTER_BOUND('',#1532,.T.);
#1061=FACE_OUTER_BOUND('',#1533,.T.);
#1062=FACE_OUTER_BOUND('',#1534,.T.);
#1063=FACE_OUTER_BOUND('',#1536,.T.);
#1064=FACE_OUTER_BOUND('',#1538,.T.);
#1065=FACE_OUTER_BOUND('',#1539,.T.);
#1066=FACE_OUTER_BOUND('',#1540,.T.);
#1067=FACE_OUTER_BOUND('',#1542,.T.);
#1068=FACE_OUTER_BOUND('',#1544,.T.);
#1069=FACE_OUTER_BOUND('',#1545,.T.);
#1070=FACE_OUTER_BOUND('',#1546,.T.);
#1071=FACE_OUTER_BOUND('',#1547,.T.);
#1072=FACE_OUTER_BOUND('',#1549,.T.);
#1073=FACE_OUTER_BOUND('',#1551,.T.);
#1074=FACE_OUTER_BOUND('',#1553,.T.);
#1075=FACE_OUTER_BOUND('',#1555,.T.);
#1076=FACE_OUTER_BOUND('',#1556,.T.);
#1077=FACE_OUTER_BOUND('',#1557,.T.);
#1078=FACE_OUTER_BOUND('',#1559,.T.);
#1079=FACE_OUTER_BOUND('',#1561,.T.);
#1080=FACE_OUTER_BOUND('',#1562,.T.);
#1081=FACE_OUTER_BOUND('',#1563,.T.);
#1082=FACE_OUTER_BOUND('',#1564,.T.);
#1083=FACE_OUTER_BOUND('',#1566,.T.);
#1084=FACE_OUTER_BOUND('',#1568,.T.);
#1085=FACE_OUTER_BOUND('',#1570,.T.);
#1086=FACE_OUTER_BOUND('',#1572,.T.);
#1087=FACE_OUTER_BOUND('',#1573,.T.);
#1088=FACE_OUTER_BOUND('',#1574,.T.);
#1089=FACE_OUTER_BOUND('',#1575,.T.);
#1090=FACE_OUTER_BOUND('',#1577,.T.);
#1091=FACE_OUTER_BOUND('',#1579,.T.);
#1092=FACE_OUTER_BOUND('',#1581,.T.);
#1093=FACE_OUTER_BOUND('',#1582,.T.);
#1094=FACE_OUTER_BOUND('',#1583,.T.);
#1095=FACE_OUTER_BOUND('',#1584,.T.);
#1096=FACE_OUTER_BOUND('',#1585,.T.);
#1097=FACE_OUTER_BOUND('',#1586,.T.);
#1098=FACE_OUTER_BOUND('',#1587,.T.);
#1099=FACE_OUTER_BOUND('',#1588,.T.);
#1100=FACE_OUTER_BOUND('',#1589,.T.);
#1101=FACE_OUTER_BOUND('',#1590,.T.);
#1102=FACE_OUTER_BOUND('',#1591,.T.);
#1103=FACE_OUTER_BOUND('',#1592,.T.);
#1104=FACE_OUTER_BOUND('',#1593,.T.);
#1105=FACE_OUTER_BOUND('',#1594,.T.);
#1106=FACE_OUTER_BOUND('',#1595,.T.);
#1107=FACE_OUTER_BOUND('',#1596,.T.);
#1108=FACE_OUTER_BOUND('',#1597,.T.);
#1109=FACE_OUTER_BOUND('',#1598,.T.);
#1110=FACE_OUTER_BOUND('',#1599,.T.);
#1111=FACE_OUTER_BOUND('',#1600,.T.);
#1112=FACE_OUTER_BOUND('',#1601,.T.);
#1113=FACE_OUTER_BOUND('',#1602,.T.);
#1114=FACE_OUTER_BOUND('',#1603,.T.);
#1115=FACE_OUTER_BOUND('',#1604,.T.);
#1116=FACE_OUTER_BOUND('',#1605,.T.);
#1117=FACE_OUTER_BOUND('',#1606,.T.);
#1118=FACE_OUTER_BOUND('',#1607,.T.);
#1119=FACE_OUTER_BOUND('',#1608,.T.);
#1120=FACE_OUTER_BOUND('',#1609,.T.);
#1121=FACE_OUTER_BOUND('',#1610,.T.);
#1122=FACE_OUTER_BOUND('',#1611,.T.);
#1123=FACE_OUTER_BOUND('',#1612,.T.);
#1124=FACE_OUTER_BOUND('',#1613,.T.);
#1125=FACE_OUTER_BOUND('',#1614,.T.);
#1126=FACE_OUTER_BOUND('',#1615,.T.);
#1127=FACE_OUTER_BOUND('',#1616,.T.);
#1128=FACE_OUTER_BOUND('',#1617,.T.);
#1129=FACE_OUTER_BOUND('',#1618,.T.);
#1130=FACE_OUTER_BOUND('',#1619,.T.);
#1131=FACE_OUTER_BOUND('',#1620,.T.);
#1132=FACE_OUTER_BOUND('',#1621,.T.);
#1133=FACE_OUTER_BOUND('',#1622,.T.);
#1134=FACE_OUTER_BOUND('',#1623,.T.);
#1135=FACE_OUTER_BOUND('',#1624,.T.);
#1136=FACE_OUTER_BOUND('',#1625,.T.);
#1137=FACE_OUTER_BOUND('',#1626,.T.);
#1138=FACE_OUTER_BOUND('',#1627,.T.);
#1139=FACE_OUTER_BOUND('',#1628,.T.);
#1140=FACE_OUTER_BOUND('',#1629,.T.);
#1141=FACE_OUTER_BOUND('',#1631,.T.);
#1142=FACE_OUTER_BOUND('',#1633,.T.);
#1143=FACE_OUTER_BOUND('',#1634,.T.);
#1144=FACE_OUTER_BOUND('',#1635,.T.);
#1145=FACE_OUTER_BOUND('',#1636,.T.);
#1146=FACE_OUTER_BOUND('',#1637,.T.);
#1147=FACE_OUTER_BOUND('',#1638,.T.);
#1148=FACE_OUTER_BOUND('',#1641,.T.);
#1149=FACE_OUTER_BOUND('',#1642,.T.);
#1150=FACE_OUTER_BOUND('',#1644,.T.);
#1151=FACE_OUTER_BOUND('',#1645,.T.);
#1152=FACE_OUTER_BOUND('',#1646,.T.);
#1153=FACE_OUTER_BOUND('',#1647,.T.);
#1154=FACE_OUTER_BOUND('',#1649,.T.);
#1155=FACE_OUTER_BOUND('',#1651,.T.);
#1156=FACE_OUTER_BOUND('',#1652,.T.);
#1157=FACE_OUTER_BOUND('',#1653,.T.);
#1158=FACE_OUTER_BOUND('',#1654,.T.);
#1159=FACE_OUTER_BOUND('',#1656,.T.);
#1160=FACE_OUTER_BOUND('',#1657,.T.);
#1161=FACE_OUTER_BOUND('',#1658,.T.);
#1162=FACE_OUTER_BOUND('',#1659,.T.);
#1163=FACE_OUTER_BOUND('',#1660,.T.);
#1164=FACE_OUTER_BOUND('',#1661,.T.);
#1165=FACE_OUTER_BOUND('',#1662,.T.);
#1166=FACE_OUTER_BOUND('',#1663,.T.);
#1167=FACE_OUTER_BOUND('',#1664,.T.);
#1168=FACE_OUTER_BOUND('',#1666,.T.);
#1169=FACE_OUTER_BOUND('',#1667,.T.);
#1170=FACE_OUTER_BOUND('',#1668,.T.);
#1171=FACE_OUTER_BOUND('',#1669,.T.);
#1172=FACE_OUTER_BOUND('',#1670,.T.);
#1173=FACE_OUTER_BOUND('',#1671,.T.);
#1174=FACE_OUTER_BOUND('',#1672,.T.);
#1175=FACE_OUTER_BOUND('',#1673,.T.);
#1176=FACE_OUTER_BOUND('',#1674,.T.);
#1177=FACE_OUTER_BOUND('',#1676,.T.);
#1178=FACE_OUTER_BOUND('',#1677,.T.);
#1179=FACE_OUTER_BOUND('',#1678,.T.);
#1180=FACE_OUTER_BOUND('',#1679,.T.);
#1181=FACE_OUTER_BOUND('',#1680,.T.);
#1182=FACE_OUTER_BOUND('',#1681,.T.);
#1183=FACE_OUTER_BOUND('',#1682,.T.);
#1184=FACE_OUTER_BOUND('',#1683,.T.);
#1185=FACE_OUTER_BOUND('',#1684,.T.);
#1186=FACE_OUTER_BOUND('',#1685,.T.);
#1187=FACE_OUTER_BOUND('',#1686,.T.);
#1188=FACE_OUTER_BOUND('',#1687,.T.);
#1189=FACE_OUTER_BOUND('',#1688,.T.);
#1190=FACE_OUTER_BOUND('',#1689,.T.);
#1191=FACE_OUTER_BOUND('',#1690,.T.);
#1192=FACE_OUTER_BOUND('',#1691,.T.);
#1193=FACE_OUTER_BOUND('',#1693,.T.);
#1194=FACE_OUTER_BOUND('',#1694,.T.);
#1195=FACE_OUTER_BOUND('',#1695,.T.);
#1196=EDGE_LOOP('',(#4247,#4248,#4249,#4250));
#1197=EDGE_LOOP('',(#4251,#4252,#4253,#4254));
#1198=EDGE_LOOP('',(#4255,#4256,#4257,#4258));
#1199=EDGE_LOOP('',(#4259,#4260,#4261,#4262));
#1200=EDGE_LOOP('',(#4263,#4264,#4265,#4266));
#1201=EDGE_LOOP('',(#4267,#4268,#4269,#4270));
#1202=EDGE_LOOP('',(#4271,#4272,#4273,#4274));
#1203=EDGE_LOOP('',(#4275,#4276,#4277,#4278));
#1204=EDGE_LOOP('',(#4279,#4280,#4281,#4282));
#1205=EDGE_LOOP('',(#4283,#4284,#4285,#4286));
#1206=EDGE_LOOP('',(#4287,#4288,#4289,#4290));
#1207=EDGE_LOOP('',(#4291,#4292,#4293,#4294));
#1208=EDGE_LOOP('',(#4295,#4296,#4297,#4298));
#1209=EDGE_LOOP('',(#4299,#4300,#4301,#4302));
#1210=EDGE_LOOP('',(#4303,#4304,#4305,#4306));
#1211=EDGE_LOOP('',(#4307));
#1212=EDGE_LOOP('',(#4308));
#1213=EDGE_LOOP('',(#4309));
#1214=EDGE_LOOP('',(#4310));
#1215=EDGE_LOOP('',(#4311));
#1216=EDGE_LOOP('',(#4312));
#1217=EDGE_LOOP('',(#4313));
#1218=EDGE_LOOP('',(#4314));
#1219=EDGE_LOOP('',(#4315));
#1220=EDGE_LOOP('',(#4316));
#1221=EDGE_LOOP('',(#4317,#4318,#4319,#4320));
#1222=EDGE_LOOP('',(#4321));
#1223=EDGE_LOOP('',(#4322));
#1224=EDGE_LOOP('',(#4323));
#1225=EDGE_LOOP('',(#4324));
#1226=EDGE_LOOP('',(#4325));
#1227=EDGE_LOOP('',(#4326));
#1228=EDGE_LOOP('',(#4327));
#1229=EDGE_LOOP('',(#4328));
#1230=EDGE_LOOP('',(#4329));
#1231=EDGE_LOOP('',(#4330));
#1232=EDGE_LOOP('',(#4331,#4332,#4333,#4334));
#1233=EDGE_LOOP('',(#4335,#4336,#4337,#4338));
#1234=EDGE_LOOP('',(#4339,#4340,#4341,#4342));
#1235=EDGE_LOOP('',(#4343,#4344,#4345,#4346));
#1236=EDGE_LOOP('',(#4347,#4348,#4349,#4350));
#1237=EDGE_LOOP('',(#4351,#4352,#4353,#4354));
#1238=EDGE_LOOP('',(#4355,#4356,#4357,#4358));
#1239=EDGE_LOOP('',(#4359,#4360,#4361,#4362));
#1240=EDGE_LOOP('',(#4363,#4364,#4365,#4366));
#1241=EDGE_LOOP('',(#4367,#4368,#4369,#4370));
#1242=EDGE_LOOP('',(#4371,#4372,#4373,#4374));
#1243=EDGE_LOOP('',(#4375,#4376,#4377,#4378));
#1244=EDGE_LOOP('',(#4379,#4380,#4381,#4382));
#1245=EDGE_LOOP('',(#4383));
#1246=EDGE_LOOP('',(#4384));
#1247=EDGE_LOOP('',(#4385,#4386,#4387,#4388));
#1248=EDGE_LOOP('',(#4389));
#1249=EDGE_LOOP('',(#4390));
#1250=EDGE_LOOP('',(#4391,#4392,#4393,#4394));
#1251=EDGE_LOOP('',(#4395,#4396,#4397,#4398));
#1252=EDGE_LOOP('',(#4399,#4400,#4401,#4402));
#1253=EDGE_LOOP('',(#4403));
#1254=EDGE_LOOP('',(#4404));
#1255=EDGE_LOOP('',(#4405,#4406,#4407,#4408));
#1256=EDGE_LOOP('',(#4409));
#1257=EDGE_LOOP('',(#4410));
#1258=EDGE_LOOP('',(#4411,#4412,#4413,#4414));
#1259=EDGE_LOOP('',(#4415,#4416,#4417,#4418));
#1260=EDGE_LOOP('',(#4419,#4420,#4421,#4422));
#1261=EDGE_LOOP('',(#4423,#4424,#4425,#4426));
#1262=EDGE_LOOP('',(#4427,#4428,#4429,#4430));
#1263=EDGE_LOOP('',(#4431,#4432,#4433,#4434));
#1264=EDGE_LOOP('',(#4435,#4436,#4437,#4438));
#1265=EDGE_LOOP('',(#4439,#4440,#4441,#4442));
#1266=EDGE_LOOP('',(#4443,#4444,#4445,#4446));
#1267=EDGE_LOOP('',(#4447));
#1268=EDGE_LOOP('',(#4448));
#1269=EDGE_LOOP('',(#4449));
#1270=EDGE_LOOP('',(#4450));
#1271=EDGE_LOOP('',(#4451));
#1272=EDGE_LOOP('',(#4452));
#1273=EDGE_LOOP('',(#4453,#4454,#4455,#4456));
#1274=EDGE_LOOP('',(#4457));
#1275=EDGE_LOOP('',(#4458));
#1276=EDGE_LOOP('',(#4459));
#1277=EDGE_LOOP('',(#4460));
#1278=EDGE_LOOP('',(#4461));
#1279=EDGE_LOOP('',(#4462));
#1280=EDGE_LOOP('',(#4463,#4464,#4465,#4466));
#1281=EDGE_LOOP('',(#4467,#4468,#4469,#4470));
#1282=EDGE_LOOP('',(#4471));
#1283=EDGE_LOOP('',(#4472));
#1284=EDGE_LOOP('',(#4473));
#1285=EDGE_LOOP('',(#4474));
#1286=EDGE_LOOP('',(#4475,#4476,#4477,#4478));
#1287=EDGE_LOOP('',(#4479,#4480,#4481,#4482));
#1288=EDGE_LOOP('',(#4483));
#1289=EDGE_LOOP('',(#4484));
#1290=EDGE_LOOP('',(#4485));
#1291=EDGE_LOOP('',(#4486));
#1292=EDGE_LOOP('',(#4487,#4488,#4489,#4490));
#1293=EDGE_LOOP('',(#4491));
#1294=EDGE_LOOP('',(#4492));
#1295=EDGE_LOOP('',(#4493,#4494,#4495,#4496));
#1296=EDGE_LOOP('',(#4497));
#1297=EDGE_LOOP('',(#4498));
#1298=EDGE_LOOP('',(#4499,#4500,#4501,#4502));
#1299=EDGE_LOOP('',(#4503,#4504,#4505,#4506));
#1300=EDGE_LOOP('',(#4507,#4508,#4509,#4510));
#1301=EDGE_LOOP('',(#4511));
#1302=EDGE_LOOP('',(#4512));
#1303=EDGE_LOOP('',(#4513,#4514,#4515,#4516));
#1304=EDGE_LOOP('',(#4517));
#1305=EDGE_LOOP('',(#4518));
#1306=EDGE_LOOP('',(#4519,#4520,#4521,#4522));
#1307=EDGE_LOOP('',(#4523,#4524,#4525,#4526));
#1308=EDGE_LOOP('',(#4527,#4528,#4529,#4530));
#1309=EDGE_LOOP('',(#4531,#4532,#4533,#4534));
#1310=EDGE_LOOP('',(#4535,#4536,#4537,#4538));
#1311=EDGE_LOOP('',(#4539,#4540,#4541,#4542));
#1312=EDGE_LOOP('',(#4543,#4544,#4545,#4546));
#1313=EDGE_LOOP('',(#4547,#4548,#4549,#4550));
#1314=EDGE_LOOP('',(#4551,#4552,#4553,#4554));
#1315=EDGE_LOOP('',(#4555));
#1316=EDGE_LOOP('',(#4556));
#1317=EDGE_LOOP('',(#4557));
#1318=EDGE_LOOP('',(#4558));
#1319=EDGE_LOOP('',(#4559));
#1320=EDGE_LOOP('',(#4560));
#1321=EDGE_LOOP('',(#4561,#4562,#4563,#4564));
#1322=EDGE_LOOP('',(#4565));
#1323=EDGE_LOOP('',(#4566));
#1324=EDGE_LOOP('',(#4567));
#1325=EDGE_LOOP('',(#4568));
#1326=EDGE_LOOP('',(#4569));
#1327=EDGE_LOOP('',(#4570));
#1328=EDGE_LOOP('',(#4571,#4572,#4573,#4574));
#1329=EDGE_LOOP('',(#4575,#4576,#4577,#4578));
#1330=EDGE_LOOP('',(#4579));
#1331=EDGE_LOOP('',(#4580));
#1332=EDGE_LOOP('',(#4581));
#1333=EDGE_LOOP('',(#4582));
#1334=EDGE_LOOP('',(#4583,#4584,#4585,#4586));
#1335=EDGE_LOOP('',(#4587,#4588,#4589,#4590));
#1336=EDGE_LOOP('',(#4591));
#1337=EDGE_LOOP('',(#4592));
#1338=EDGE_LOOP('',(#4593));
#1339=EDGE_LOOP('',(#4594));
#1340=EDGE_LOOP('',(#4595,#4596,#4597,#4598));
#1341=EDGE_LOOP('',(#4599,#4600,#4601,#4602));
#1342=EDGE_LOOP('',(#4603,#4604,#4605,#4606));
#1343=EDGE_LOOP('',(#4607,#4608,#4609,#4610));
#1344=EDGE_LOOP('',(#4611));
#1345=EDGE_LOOP('',(#4612));
#1346=EDGE_LOOP('',(#4613,#4614,#4615,#4616));
#1347=EDGE_LOOP('',(#4617,#4618,#4619,#4620));
#1348=EDGE_LOOP('',(#4621,#4622,#4623,#4624));
#1349=EDGE_LOOP('',(#4625,#4626,#4627,#4628));
#1350=EDGE_LOOP('',(#4629,#4630,#4631,#4632));
#1351=EDGE_LOOP('',(#4633,#4634,#4635,#4636));
#1352=EDGE_LOOP('',(#4637));
#1353=EDGE_LOOP('',(#4638,#4639,#4640,#4641));
#1354=EDGE_LOOP('',(#4642,#4643,#4644,#4645));
#1355=EDGE_LOOP('',(#4646));
#1356=EDGE_LOOP('',(#4647,#4648,#4649,#4650));
#1357=EDGE_LOOP('',(#4651,#4652,#4653,#4654));
#1358=EDGE_LOOP('',(#4655,#4656,#4657,#4658));
#1359=EDGE_LOOP('',(#4659));
#1360=EDGE_LOOP('',(#4660));
#1361=EDGE_LOOP('',(#4661,#4662,#4663,#4664));
#1362=EDGE_LOOP('',(#4665));
#1363=EDGE_LOOP('',(#4666));
#1364=EDGE_LOOP('',(#4667));
#1365=EDGE_LOOP('',(#4668,#4669,#4670,#4671));
#1366=EDGE_LOOP('',(#4672));
#1367=EDGE_LOOP('',(#4673,#4674,#4675,#4676));
#1368=EDGE_LOOP('',(#4677));
#1369=EDGE_LOOP('',(#4678));
#1370=EDGE_LOOP('',(#4679,#4680,#4681,#4682));
#1371=EDGE_LOOP('',(#4683,#4684,#4685,#4686));
#1372=EDGE_LOOP('',(#4687));
#1373=EDGE_LOOP('',(#4688));
#1374=EDGE_LOOP('',(#4689));
#1375=EDGE_LOOP('',(#4690));
#1376=EDGE_LOOP('',(#4691,#4692,#4693,#4694));
#1377=EDGE_LOOP('',(#4695,#4696,#4697,#4698));
#1378=EDGE_LOOP('',(#4699));
#1379=EDGE_LOOP('',(#4700));
#1380=EDGE_LOOP('',(#4701));
#1381=EDGE_LOOP('',(#4702));
#1382=EDGE_LOOP('',(#4703,#4704,#4705,#4706));
#1383=EDGE_LOOP('',(#4707,#4708,#4709,#4710));
#1384=EDGE_LOOP('',(#4711,#4712,#4713,#4714));
#1385=EDGE_LOOP('',(#4715,#4716,#4717,#4718));
#1386=EDGE_LOOP('',(#4719,#4720,#4721,#4722));
#1387=EDGE_LOOP('',(#4723,#4724,#4725,#4726));
#1388=EDGE_LOOP('',(#4727,#4728,#4729,#4730));
#1389=EDGE_LOOP('',(#4731,#4732,#4733,#4734));
#1390=EDGE_LOOP('',(#4735,#4736,#4737,#4738));
#1391=EDGE_LOOP('',(#4739,#4740,#4741,#4742));
#1392=EDGE_LOOP('',(#4743,#4744,#4745,#4746));
#1393=EDGE_LOOP('',(#4747,#4748,#4749,#4750));
#1394=EDGE_LOOP('',(#4751));
#1395=EDGE_LOOP('',(#4752,#4753,#4754,#4755));
#1396=EDGE_LOOP('',(#4756));
#1397=EDGE_LOOP('',(#4757,#4758,#4759,#4760));
#1398=EDGE_LOOP('',(#4761,#4762,#4763,#4764));
#1399=EDGE_LOOP('',(#4765,#4766));
#1400=EDGE_LOOP('',(#4767));
#1401=EDGE_LOOP('',(#4768));
#1402=EDGE_LOOP('',(#4769,#4770,#4771));
#1403=EDGE_LOOP('',(#4772,#4773,#4774));
#1404=EDGE_LOOP('',(#4775,#4776,#4777));
#1405=EDGE_LOOP('',(#4778,#4779,#4780,#4781));
#1406=EDGE_LOOP('',(#4782,#4783,#4784));
#1407=EDGE_LOOP('',(#4785,#4786,#4787,#4788));
#1408=EDGE_LOOP('',(#4789,#4790,#4791,#4792));
#1409=EDGE_LOOP('',(#4793));
#1410=EDGE_LOOP('',(#4794));
#1411=EDGE_LOOP('',(#4795,#4796,#4797,#4798,#4799,#4800,#4801,#4802,#4803,
#4804,#4805,#4806));
#1412=EDGE_LOOP('',(#4807,#4808,#4809,#4810,#4811,#4812,#4813,#4814,#4815,
#4816,#4817,#4818));
#1413=EDGE_LOOP('',(#4819,#4820));
#1414=EDGE_LOOP('',(#4821));
#1415=EDGE_LOOP('',(#4822,#4823));
#1416=EDGE_LOOP('',(#4824));
#1417=EDGE_LOOP('',(#4825,#4826,#4827,#4828));
#1418=EDGE_LOOP('',(#4829,#4830,#4831,#4832));
#1419=EDGE_LOOP('',(#4833,#4834,#4835,#4836));
#1420=EDGE_LOOP('',(#4837,#4838,#4839,#4840));
#1421=EDGE_LOOP('',(#4841,#4842,#4843,#4844));
#1422=EDGE_LOOP('',(#4845,#4846,#4847,#4848));
#1423=EDGE_LOOP('',(#4849,#4850,#4851,#4852));
#1424=EDGE_LOOP('',(#4853,#4854,#4855,#4856));
#1425=EDGE_LOOP('',(#4857,#4858,#4859,#4860));
#1426=EDGE_LOOP('',(#4861,#4862,#4863,#4864));
#1427=EDGE_LOOP('',(#4865,#4866,#4867,#4868));
#1428=EDGE_LOOP('',(#4869,#4870,#4871,#4872));
#1429=EDGE_LOOP('',(#4873,#4874,#4875,#4876));
#1430=EDGE_LOOP('',(#4877));
#1431=EDGE_LOOP('',(#4878));
#1432=EDGE_LOOP('',(#4879,#4880,#4881,#4882));
#1433=EDGE_LOOP('',(#4883));
#1434=EDGE_LOOP('',(#4884));
#1435=EDGE_LOOP('',(#4885,#4886));
#1436=EDGE_LOOP('',(#4887));
#1437=EDGE_LOOP('',(#4888));
#1438=EDGE_LOOP('',(#4889));
#1439=EDGE_LOOP('',(#4890));
#1440=EDGE_LOOP('',(#4891,#4892,#4893,#4894,#4895,#4896));
#1441=EDGE_LOOP('',(#4897,#4898,#4899,#4900,#4901,#4902));
#1442=EDGE_LOOP('',(#4903,#4904,#4905,#4906));
#1443=EDGE_LOOP('',(#4907,#4908,#4909));
#1444=EDGE_LOOP('',(#4910,#4911,#4912));
#1445=EDGE_LOOP('',(#4913,#4914,#4915));
#1446=EDGE_LOOP('',(#4916,#4917,#4918));
#1447=EDGE_LOOP('',(#4919,#4920,#4921));
#1448=EDGE_LOOP('',(#4922,#4923,#4924));
#1449=EDGE_LOOP('',(#4925,#4926,#4927,#4928,#4929,#4930));
#1450=EDGE_LOOP('',(#4931,#4932,#4933,#4934,#4935,#4936));
#1451=EDGE_LOOP('',(#4937,#4938,#4939,#4940,#4941,#4942));
#1452=EDGE_LOOP('',(#4943,#4944,#4945,#4946,#4947,#4948));
#1453=EDGE_LOOP('',(#4949));
#1454=EDGE_LOOP('',(#4950));
#1455=EDGE_LOOP('',(#4951));
#1456=EDGE_LOOP('',(#4952));
#1457=EDGE_LOOP('',(#4953,#4954,#4955,#4956));
#1458=EDGE_LOOP('',(#4957));
#1459=EDGE_LOOP('',(#4958));
#1460=EDGE_LOOP('',(#4959,#4960,#4961,#4962));
#1461=EDGE_LOOP('',(#4963));
#1462=EDGE_LOOP('',(#4964));
#1463=EDGE_LOOP('',(#4965));
#1464=EDGE_LOOP('',(#4966));
#1465=EDGE_LOOP('',(#4967));
#1466=EDGE_LOOP('',(#4968));
#1467=EDGE_LOOP('',(#4969,#4970,#4971,#4972));
#1468=EDGE_LOOP('',(#4973,#4974,#4975,#4976));
#1469=EDGE_LOOP('',(#4977));
#1470=EDGE_LOOP('',(#4978));
#1471=EDGE_LOOP('',(#4979));
#1472=EDGE_LOOP('',(#4980));
#1473=EDGE_LOOP('',(#4981,#4982,#4983,#4984));
#1474=EDGE_LOOP('',(#4985,#4986,#4987,#4988));
#1475=EDGE_LOOP('',(#4989,#4990,#4991,#4992));
#1476=EDGE_LOOP('',(#4993,#4994,#4995,#4996));
#1477=EDGE_LOOP('',(#4997,#4998,#4999,#5000));
#1478=EDGE_LOOP('',(#5001,#5002,#5003,#5004));
#1479=EDGE_LOOP('',(#5005,#5006,#5007,#5008,#5009,#5010));
#1480=EDGE_LOOP('',(#5011,#5012,#5013,#5014,#5015,#5016));
#1481=EDGE_LOOP('',(#5017));
#1482=EDGE_LOOP('',(#5018));
#1483=EDGE_LOOP('',(#5019,#5020,#5021,#5022));
#1484=EDGE_LOOP('',(#5023,#5024,#5025,#5026));
#1485=EDGE_LOOP('',(#5027,#5028,#5029,#5030));
#1486=EDGE_LOOP('',(#5031));
#1487=EDGE_LOOP('',(#5032));
#1488=EDGE_LOOP('',(#5033,#5034,#5035,#5036));
#1489=EDGE_LOOP('',(#5037,#5038,#5039,#5040));
#1490=EDGE_LOOP('',(#5041,#5042,#5043,#5044));
#1491=EDGE_LOOP('',(#5045,#5046,#5047,#5048));
#1492=EDGE_LOOP('',(#5049,#5050,#5051,#5052));
#1493=EDGE_LOOP('',(#5053,#5054,#5055,#5056));
#1494=EDGE_LOOP('',(#5057,#5058,#5059,#5060));
#1495=EDGE_LOOP('',(#5061,#5062,#5063,#5064));
#1496=EDGE_LOOP('',(#5065,#5066,#5067,#5068,#5069,#5070));
#1497=EDGE_LOOP('',(#5071,#5072,#5073,#5074,#5075,#5076));
#1498=EDGE_LOOP('',(#5077));
#1499=EDGE_LOOP('',(#5078));
#1500=EDGE_LOOP('',(#5079,#5080,#5081,#5082));
#1501=EDGE_LOOP('',(#5083,#5084,#5085,#5086));
#1502=EDGE_LOOP('',(#5087,#5088,#5089,#5090));
#1503=EDGE_LOOP('',(#5091));
#1504=EDGE_LOOP('',(#5092));
#1505=EDGE_LOOP('',(#5093,#5094,#5095,#5096));
#1506=EDGE_LOOP('',(#5097,#5098,#5099,#5100));
#1507=EDGE_LOOP('',(#5101,#5102,#5103,#5104));
#1508=EDGE_LOOP('',(#5105));
#1509=EDGE_LOOP('',(#5106));
#1510=EDGE_LOOP('',(#5107,#5108));
#1511=EDGE_LOOP('',(#5109,#5110,#5111,#5112,#5113,#5114,#5115,#5116,#5117));
#1512=EDGE_LOOP('',(#5118,#5119,#5120));
#1513=EDGE_LOOP('',(#5121,#5122,#5123,#5124));
#1514=EDGE_LOOP('',(#5125,#5126,#5127,#5128));
#1515=EDGE_LOOP('',(#5129,#5130,#5131,#5132));
#1516=EDGE_LOOP('',(#5133,#5134));
#1517=EDGE_LOOP('',(#5135));
#1518=EDGE_LOOP('',(#5136));
#1519=EDGE_LOOP('',(#5137));
#1520=EDGE_LOOP('',(#5138));
#1521=EDGE_LOOP('',(#5139,#5140));
#1522=EDGE_LOOP('',(#5141,#5142,#5143,#5144,#5145,#5146,#5147,#5148,#5149));
#1523=EDGE_LOOP('',(#5150,#5151,#5152));
#1524=EDGE_LOOP('',(#5153,#5154,#5155,#5156));
#1525=EDGE_LOOP('',(#5157,#5158,#5159,#5160));
#1526=EDGE_LOOP('',(#5161,#5162,#5163,#5164));
#1527=EDGE_LOOP('',(#5165,#5166));
#1528=EDGE_LOOP('',(#5167));
#1529=EDGE_LOOP('',(#5168));
#1530=EDGE_LOOP('',(#5169));
#1531=EDGE_LOOP('',(#5170));
#1532=EDGE_LOOP('',(#5171,#5172,#5173,#5174));
#1533=EDGE_LOOP('',(#5175,#5176,#5177,#5178));
#1534=EDGE_LOOP('',(#5179));
#1535=EDGE_LOOP('',(#5180));
#1536=EDGE_LOOP('',(#5181));
#1537=EDGE_LOOP('',(#5182));
#1538=EDGE_LOOP('',(#5183,#5184,#5185,#5186));
#1539=EDGE_LOOP('',(#5187,#5188,#5189,#5190));
#1540=EDGE_LOOP('',(#5191));
#1541=EDGE_LOOP('',(#5192));
#1542=EDGE_LOOP('',(#5193));
#1543=EDGE_LOOP('',(#5194));
#1544=EDGE_LOOP('',(#5195,#5196));
#1545=EDGE_LOOP('',(#5197,#5198,#5199,#5200,#5201,#5202,#5203,#5204,#5205));
#1546=EDGE_LOOP('',(#5206,#5207,#5208));
#1547=EDGE_LOOP('',(#5209,#5210,#5211,#5212));
#1548=EDGE_LOOP('',(#5213,#5214,#5215,#5216));
#1549=EDGE_LOOP('',(#5217,#5218,#5219,#5220));
#1550=EDGE_LOOP('',(#5221,#5222));
#1551=EDGE_LOOP('',(#5223));
#1552=EDGE_LOOP('',(#5224));
#1553=EDGE_LOOP('',(#5225));
#1554=EDGE_LOOP('',(#5226));
#1555=EDGE_LOOP('',(#5227,#5228,#5229,#5230));
#1556=EDGE_LOOP('',(#5231,#5232,#5233,#5234));
#1557=EDGE_LOOP('',(#5235));
#1558=EDGE_LOOP('',(#5236));
#1559=EDGE_LOOP('',(#5237));
#1560=EDGE_LOOP('',(#5238));
#1561=EDGE_LOOP('',(#5239,#5240));
#1562=EDGE_LOOP('',(#5241,#5242,#5243,#5244,#5245,#5246,#5247,#5248,#5249));
#1563=EDGE_LOOP('',(#5250,#5251,#5252));
#1564=EDGE_LOOP('',(#5253,#5254,#5255,#5256));
#1565=EDGE_LOOP('',(#5257,#5258,#5259,#5260));
#1566=EDGE_LOOP('',(#5261,#5262,#5263,#5264));
#1567=EDGE_LOOP('',(#5265,#5266));
#1568=EDGE_LOOP('',(#5267));
#1569=EDGE_LOOP('',(#5268));
#1570=EDGE_LOOP('',(#5269));
#1571=EDGE_LOOP('',(#5270));
#1572=EDGE_LOOP('',(#5271,#5272));
#1573=EDGE_LOOP('',(#5273,#5274,#5275,#5276,#5277,#5278,#5279,#5280,#5281));
#1574=EDGE_LOOP('',(#5282,#5283,#5284));
#1575=EDGE_LOOP('',(#5285,#5286,#5287,#5288));
#1576=EDGE_LOOP('',(#5289,#5290));
#1577=EDGE_LOOP('',(#5291));
#1578=EDGE_LOOP('',(#5292));
#1579=EDGE_LOOP('',(#5293,#5294,#5295,#5296));
#1580=EDGE_LOOP('',(#5297,#5298,#5299,#5300));
#1581=EDGE_LOOP('',(#5301,#5302,#5303,#5304));
#1582=EDGE_LOOP('',(#5305,#5306,#5307,#5308));
#1583=EDGE_LOOP('',(#5309,#5310,#5311,#5312));
#1584=EDGE_LOOP('',(#5313,#5314,#5315,#5316));
#1585=EDGE_LOOP('',(#5317,#5318,#5319,#5320));
#1586=EDGE_LOOP('',(#5321,#5322,#5323,#5324));
#1587=EDGE_LOOP('',(#5325,#5326,#5327,#5328));
#1588=EDGE_LOOP('',(#5329,#5330,#5331,#5332));
#1589=EDGE_LOOP('',(#5333,#5334,#5335,#5336));
#1590=EDGE_LOOP('',(#5337,#5338,#5339,#5340));
#1591=EDGE_LOOP('',(#5341,#5342,#5343,#5344));
#1592=EDGE_LOOP('',(#5345,#5346,#5347,#5348));
#1593=EDGE_LOOP('',(#5349,#5350,#5351,#5352));
#1594=EDGE_LOOP('',(#5353,#5354,#5355,#5356));
#1595=EDGE_LOOP('',(#5357,#5358,#5359,#5360));
#1596=EDGE_LOOP('',(#5361,#5362,#5363,#5364));
#1597=EDGE_LOOP('',(#5365,#5366,#5367,#5368));
#1598=EDGE_LOOP('',(#5369,#5370,#5371,#5372));
#1599=EDGE_LOOP('',(#5373,#5374,#5375,#5376));
#1600=EDGE_LOOP('',(#5377,#5378,#5379,#5380));
#1601=EDGE_LOOP('',(#5381,#5382,#5383,#5384));
#1602=EDGE_LOOP('',(#5385,#5386,#5387,#5388));
#1603=EDGE_LOOP('',(#5389,#5390,#5391,#5392));
#1604=EDGE_LOOP('',(#5393,#5394,#5395,#5396));
#1605=EDGE_LOOP('',(#5397,#5398,#5399,#5400));
#1606=EDGE_LOOP('',(#5401,#5402,#5403,#5404));
#1607=EDGE_LOOP('',(#5405,#5406,#5407,#5408));
#1608=EDGE_LOOP('',(#5409,#5410,#5411,#5412));
#1609=EDGE_LOOP('',(#5413,#5414,#5415,#5416));
#1610=EDGE_LOOP('',(#5417,#5418,#5419,#5420));
#1611=EDGE_LOOP('',(#5421,#5422,#5423,#5424));
#1612=EDGE_LOOP('',(#5425,#5426,#5427,#5428));
#1613=EDGE_LOOP('',(#5429,#5430,#5431,#5432));
#1614=EDGE_LOOP('',(#5433,#5434,#5435,#5436));
#1615=EDGE_LOOP('',(#5437,#5438,#5439,#5440));
#1616=EDGE_LOOP('',(#5441,#5442,#5443,#5444));
#1617=EDGE_LOOP('',(#5445,#5446,#5447,#5448));
#1618=EDGE_LOOP('',(#5449,#5450,#5451,#5452));
#1619=EDGE_LOOP('',(#5453,#5454,#5455,#5456));
#1620=EDGE_LOOP('',(#5457,#5458,#5459,#5460));
#1621=EDGE_LOOP('',(#5461,#5462,#5463,#5464));
#1622=EDGE_LOOP('',(#5465,#5466,#5467,#5468));
#1623=EDGE_LOOP('',(#5469,#5470,#5471,#5472));
#1624=EDGE_LOOP('',(#5473,#5474,#5475,#5476));
#1625=EDGE_LOOP('',(#5477,#5478,#5479,#5480));
#1626=EDGE_LOOP('',(#5481,#5482,#5483,#5484));
#1627=EDGE_LOOP('',(#5485,#5486,#5487,#5488));
#1628=EDGE_LOOP('',(#5489,#5490,#5491,#5492));
#1629=EDGE_LOOP('',(#5493,#5494,#5495,#5496,#5497,#5498,#5499,#5500,#5501,
#5502,#5503,#5504,#5505,#5506,#5507,#5508,#5509,#5510,#5511,#5512,#5513,
#5514,#5515,#5516,#5517,#5518,#5519,#5520,#5521,#5522,#5523,#5524,#5525,
#5526,#5527,#5528,#5529,#5530,#5531,#5532,#5533,#5534,#5535,#5536,#5537,
#5538,#5539,#5540));
#1630=EDGE_LOOP('',(#5541));
#1631=EDGE_LOOP('',(#5542,#5543,#5544,#5545,#5546,#5547,#5548,#5549,#5550,
#5551,#5552,#5553,#5554,#5555,#5556,#5557,#5558,#5559,#5560,#5561,#5562,
#5563,#5564,#5565,#5566,#5567,#5568,#5569,#5570,#5571,#5572,#5573,#5574,
#5575,#5576,#5577,#5578,#5579,#5580,#5581,#5582,#5583,#5584,#5585,#5586,
#5587,#5588,#5589));
#1632=EDGE_LOOP('',(#5590));
#1633=EDGE_LOOP('',(#5591,#5592,#5593,#5594));
#1634=EDGE_LOOP('',(#5595,#5596));
#1635=EDGE_LOOP('',(#5597,#5598,#5599,#5600,#5601,#5602,#5603,#5604));
#1636=EDGE_LOOP('',(#5605));
#1637=EDGE_LOOP('',(#5606,#5607,#5608));
#1638=EDGE_LOOP('',(#5609,#5610,#5611,#5612,#5613));
#1639=EDGE_LOOP('',(#5614));
#1640=EDGE_LOOP('',(#5615));
#1641=EDGE_LOOP('',(#5616,#5617,#5618,#5619));
#1642=EDGE_LOOP('',(#5620,#5621,#5622,#5623));
#1643=EDGE_LOOP('',(#5624));
#1644=EDGE_LOOP('',(#5625,#5626,#5627,#5628));
#1645=EDGE_LOOP('',(#5629,#5630,#5631,#5632));
#1646=EDGE_LOOP('',(#5633,#5634,#5635,#5636,#5637,#5638,#5639,#5640));
#1647=EDGE_LOOP('',(#5641,#5642,#5643,#5644));
#1648=EDGE_LOOP('',(#5645,#5646,#5647,#5648));
#1649=EDGE_LOOP('',(#5649));
#1650=EDGE_LOOP('',(#5650));
#1651=EDGE_LOOP('',(#5651,#5652,#5653,#5654));
#1652=EDGE_LOOP('',(#5655));
#1653=EDGE_LOOP('',(#5656,#5657,#5658,#5659));
#1654=EDGE_LOOP('',(#5660));
#1655=EDGE_LOOP('',(#5661));
#1656=EDGE_LOOP('',(#5662));
#1657=EDGE_LOOP('',(#5663,#5664,#5665,#5666));
#1658=EDGE_LOOP('',(#5667,#5668,#5669,#5670));
#1659=EDGE_LOOP('',(#5671,#5672,#5673,#5674));
#1660=EDGE_LOOP('',(#5675,#5676,#5677,#5678));
#1661=EDGE_LOOP('',(#5679,#5680,#5681,#5682));
#1662=EDGE_LOOP('',(#5683,#5684,#5685,#5686));
#1663=EDGE_LOOP('',(#5687,#5688,#5689,#5690,#5691,#5692));
#1664=EDGE_LOOP('',(#5693));
#1665=EDGE_LOOP('',(#5694,#5695,#5696,#5697,#5698,#5699));
#1666=EDGE_LOOP('',(#5700,#5701,#5702,#5703));
#1667=EDGE_LOOP('',(#5704,#5705,#5706,#5707));
#1668=EDGE_LOOP('',(#5708,#5709,#5710,#5711));
#1669=EDGE_LOOP('',(#5712));
#1670=EDGE_LOOP('',(#5713));
#1671=EDGE_LOOP('',(#5714,#5715,#5716,#5717));
#1672=EDGE_LOOP('',(#5718,#5719,#5720,#5721));
#1673=EDGE_LOOP('',(#5722,#5723,#5724,#5725));
#1674=EDGE_LOOP('',(#5726));
#1675=EDGE_LOOP('',(#5727));
#1676=EDGE_LOOP('',(#5728,#5729,#5730,#5731));
#1677=EDGE_LOOP('',(#5732,#5733,#5734,#5735));
#1678=EDGE_LOOP('',(#5736,#5737,#5738,#5739));
#1679=EDGE_LOOP('',(#5740));
#1680=EDGE_LOOP('',(#5741,#5742,#5743,#5744));
#1681=EDGE_LOOP('',(#5745,#5746,#5747,#5748));
#1682=EDGE_LOOP('',(#5749,#5750,#5751,#5752));
#1683=EDGE_LOOP('',(#5753,#5754,#5755,#5756));
#1684=EDGE_LOOP('',(#5757,#5758,#5759,#5760));
#1685=EDGE_LOOP('',(#5761,#5762,#5763,#5764));
#1686=EDGE_LOOP('',(#5765,#5766,#5767,#5768,#5769,#5770));
#1687=EDGE_LOOP('',(#5771,#5772,#5773,#5774,#5775,#5776));
#1688=EDGE_LOOP('',(#5777,#5778,#5779,#5780));
#1689=EDGE_LOOP('',(#5781,#5782,#5783,#5784));
#1690=EDGE_LOOP('',(#5785,#5786,#5787,#5788));
#1691=EDGE_LOOP('',(#5789,#5790,#5791,#5792));
#1692=EDGE_LOOP('',(#5793));
#1693=EDGE_LOOP('',(#5794,#5795,#5796,#5797));
#1694=EDGE_LOOP('',(#5798,#5799,#5800,#5801));
#1695=EDGE_LOOP('',(#5802,#5803,#5804,#5805));
#1696=EDGE_LOOP('',(#5806));
#1697=LINE('',#9234,#2208);
#1698=LINE('',#9240,#2209);
#1699=LINE('',#9246,#2210);
#1700=LINE('',#9252,#2211);
#1701=LINE('',#9258,#2212);
#1702=LINE('',#9264,#2213);
#1703=LINE('',#9270,#2214);
#1704=LINE('',#9276,#2215);
#1705=LINE('',#9282,#2216);
#1706=LINE('',#9288,#2217);
#1707=LINE('',#9293,#2218);
#1708=LINE('',#9295,#2219);
#1709=LINE('',#9297,#2220);
#1710=LINE('',#9298,#2221);
#1711=LINE('',#9301,#2222);
#1712=LINE('',#9303,#2223);
#1713=LINE('',#9304,#2224);
#1714=LINE('',#9307,#2225);
#1715=LINE('',#9309,#2226);
#1716=LINE('',#9310,#2227);
#1717=LINE('',#9312,#2228);
#1718=LINE('',#9313,#2229);
#1719=LINE('',#9320,#2230);
#1720=LINE('',#9322,#2231);
#1721=LINE('',#9324,#2232);
#1722=LINE('',#9325,#2233);
#1723=LINE('',#9328,#2234);
#1724=LINE('',#9330,#2235);
#1725=LINE('',#9331,#2236);
#1726=LINE('',#9334,#2237);
#1727=LINE('',#9336,#2238);
#1728=LINE('',#9337,#2239);
#1729=LINE('',#9339,#2240);
#1730=LINE('',#9340,#2241);
#1731=LINE('',#9347,#2242);
#1732=LINE('',#9349,#2243);
#1733=LINE('',#9351,#2244);
#1734=LINE('',#9352,#2245);
#1735=LINE('',#9355,#2246);
#1736=LINE('',#9357,#2247);
#1737=LINE('',#9358,#2248);
#1738=LINE('',#9361,#2249);
#1739=LINE('',#9363,#2250);
#1740=LINE('',#9364,#2251);
#1741=LINE('',#9366,#2252);
#1742=LINE('',#9367,#2253);
#1743=LINE('',#9375,#2254);
#1744=LINE('',#9384,#2255);
#1745=LINE('',#9392,#2256);
#1746=LINE('',#9396,#2257);
#1747=LINE('',#9401,#2258);
#1748=LINE('',#9410,#2259);
#1749=LINE('',#9418,#2260);
#1750=LINE('',#9422,#2261);
#1751=LINE('',#9427,#2262);
#1752=LINE('',#9433,#2263);
#1753=LINE('',#9438,#2264);
#1754=LINE('',#9440,#2265);
#1755=LINE('',#9442,#2266);
#1756=LINE('',#9443,#2267);
#1757=LINE('',#9446,#2268);
#1758=LINE('',#9448,#2269);
#1759=LINE('',#9449,#2270);
#1760=LINE('',#9452,#2271);
#1761=LINE('',#9454,#2272);
#1762=LINE('',#9455,#2273);
#1763=LINE('',#9457,#2274);
#1764=LINE('',#9458,#2275);
#1765=LINE('',#9466,#2276);
#1766=LINE('',#9472,#2277);
#1767=LINE('',#9481,#2278);
#1768=LINE('',#9487,#2279);
#1769=LINE('',#9496,#2280);
#1770=LINE('',#9505,#2281);
#1771=LINE('',#9513,#2282);
#1772=LINE('',#9517,#2283);
#1773=LINE('',#9522,#2284);
#1774=LINE('',#9531,#2285);
#1775=LINE('',#9539,#2286);
#1776=LINE('',#9543,#2287);
#1777=LINE('',#9548,#2288);
#1778=LINE('',#9554,#2289);
#1779=LINE('',#9559,#2290);
#1780=LINE('',#9561,#2291);
#1781=LINE('',#9563,#2292);
#1782=LINE('',#9564,#2293);
#1783=LINE('',#9567,#2294);
#1784=LINE('',#9569,#2295);
#1785=LINE('',#9570,#2296);
#1786=LINE('',#9573,#2297);
#1787=LINE('',#9575,#2298);
#1788=LINE('',#9576,#2299);
#1789=LINE('',#9578,#2300);
#1790=LINE('',#9579,#2301);
#1791=LINE('',#9587,#2302);
#1792=LINE('',#9593,#2303);
#1793=LINE('',#9602,#2304);
#1794=LINE('',#9608,#2305);
#1795=LINE('',#9617,#2306);
#1796=LINE('',#9623,#2307);
#1797=LINE('',#9629,#2308);
#1798=LINE('',#9634,#2309);
#1799=LINE('',#9636,#2310);
#1800=LINE('',#9638,#2311);
#1801=LINE('',#9639,#2312);
#1802=LINE('',#9642,#2313);
#1803=LINE('',#9644,#2314);
#1804=LINE('',#9646,#2315);
#1805=LINE('',#9647,#2316);
#1806=LINE('',#9650,#2317);
#1807=LINE('',#9652,#2318);
#1808=LINE('',#9653,#2319);
#1809=LINE('',#9656,#2320);
#1810=LINE('',#9658,#2321);
#1811=LINE('',#9659,#2322);
#1812=LINE('',#9661,#2323);
#1813=LINE('',#9663,#2324);
#1814=LINE('',#9666,#2325);
#1815=LINE('',#9668,#2326);
#1816=LINE('',#9669,#2327);
#1817=LINE('',#9672,#2328);
#1818=LINE('',#9673,#2329);
#1819=LINE('',#9676,#2330);
#1820=LINE('',#9677,#2331);
#1821=LINE('',#9679,#2332);
#1822=LINE('',#9687,#2333);
#1823=LINE('',#9697,#2334);
#1824=LINE('',#9703,#2335);
#1825=LINE('',#9710,#2336);
#1826=LINE('',#9716,#2337);
#1827=LINE('',#9725,#2338);
#1828=LINE('',#9731,#2339);
#1829=LINE('',#9739,#2340);
#1830=LINE('',#9741,#2341);
#1831=LINE('',#9743,#2342);
#1832=LINE('',#9744,#2343);
#1833=LINE('',#9747,#2344);
#1834=LINE('',#9749,#2345);
#1835=LINE('',#9750,#2346);
#1836=LINE('',#9753,#2347);
#1837=LINE('',#9755,#2348);
#1838=LINE('',#9756,#2349);
#1839=LINE('',#9758,#2350);
#1840=LINE('',#9759,#2351);
#1841=LINE('',#9767,#2352);
#1842=LINE('',#9772,#2353);
#1843=LINE('',#9774,#2354);
#1844=LINE('',#9776,#2355);
#1845=LINE('',#9777,#2356);
#1846=LINE('',#9780,#2357);
#1847=LINE('',#9782,#2358);
#1848=LINE('',#9783,#2359);
#1849=LINE('',#9786,#2360);
#1850=LINE('',#9788,#2361);
#1851=LINE('',#9789,#2362);
#1852=LINE('',#9791,#2363);
#1853=LINE('',#9792,#2364);
#1854=LINE('',#9801,#2365);
#1855=LINE('',#9807,#2366);
#1856=LINE('',#9816,#2367);
#1857=LINE('',#9818,#2368);
#1858=LINE('',#9823,#2369);
#1859=LINE('',#9826,#2370);
#1860=LINE('',#9830,#2371);
#1861=LINE('',#9833,#2372);
#1862=LINE('',#9835,#2373);
#1863=LINE('',#9836,#2374);
#1864=LINE('',#9840,#2375);
#1865=LINE('',#9842,#2376);
#1866=LINE('',#9845,#2377);
#1867=LINE('',#9846,#2378);
#1868=LINE('',#9850,#2379);
#1869=LINE('',#9852,#2380);
#1870=LINE('',#9854,#2381);
#1871=LINE('',#9855,#2382);
#1872=LINE('',#9861,#2383);
#1873=LINE('',#9863,#2384);
#1874=LINE('',#9864,#2385);
#1875=LINE('',#9866,#2386);
#1876=LINE('',#9868,#2387);
#1877=LINE('',#9869,#2388);
#1878=LINE('',#9878,#2389);
#1879=LINE('',#9880,#2390);
#1880=LINE('',#9882,#2391);
#1881=LINE('',#9883,#2392);
#1882=LINE('',#9886,#2393);
#1883=LINE('',#9888,#2394);
#1884=LINE('',#9889,#2395);
#1885=LINE('',#9892,#2396);
#1886=LINE('',#9894,#2397);
#1887=LINE('',#9895,#2398);
#1888=LINE('',#9897,#2399);
#1889=LINE('',#9898,#2400);
#1890=LINE('',#9903,#2401);
#1891=LINE('',#9907,#2402);
#1892=LINE('',#9911,#2403);
#1893=LINE('',#9912,#2404);
#1894=LINE('',#9913,#2405);
#1895=LINE('',#9916,#2406);
#1896=LINE('',#9917,#2407);
#1897=LINE('',#9920,#2408);
#1898=LINE('',#9921,#2409);
#1899=LINE('',#9923,#2410);
#1900=LINE('',#9930,#2411);
#1901=LINE('',#9985,#2412);
#1902=LINE('',#10057,#2413);
#1903=LINE('',#10102,#2414);
#1904=LINE('',#10270,#2415);
#1905=LINE('',#10341,#2416);
#1906=LINE('',#10344,#2417);
#1907=LINE('',#10415,#2418);
#1908=LINE('',#10425,#2419);
#1909=LINE('',#10430,#2420);
#1910=LINE('',#10438,#2421);
#1911=LINE('',#10444,#2422);
#1912=LINE('',#10452,#2423);
#1913=LINE('',#10454,#2424);
#1914=LINE('',#10456,#2425);
#1915=LINE('',#10457,#2426);
#1916=LINE('',#10460,#2427);
#1917=LINE('',#10462,#2428);
#1918=LINE('',#10463,#2429);
#1919=LINE('',#10466,#2430);
#1920=LINE('',#10468,#2431);
#1921=LINE('',#10469,#2432);
#1922=LINE('',#10472,#2433);
#1923=LINE('',#10474,#2434);
#1924=LINE('',#10475,#2435);
#1925=LINE('',#10478,#2436);
#1926=LINE('',#10480,#2437);
#1927=LINE('',#10481,#2438);
#1928=LINE('',#10483,#2439);
#1929=LINE('',#10484,#2440);
#1930=LINE('',#10496,#2441);
#1931=LINE('',#10500,#2442);
#1932=LINE('',#10504,#2443);
#1933=LINE('',#10511,#2444);
#1934=LINE('',#10513,#2445);
#1935=LINE('',#10518,#2446);
#1936=LINE('',#10520,#2447);
#1937=LINE('',#10522,#2448);
#1938=LINE('',#10523,#2449);
#1939=LINE('',#10526,#2450);
#1940=LINE('',#10528,#2451);
#1941=LINE('',#10529,#2452);
#1942=LINE('',#10532,#2453);
#1943=LINE('',#10534,#2454);
#1944=LINE('',#10535,#2455);
#1945=LINE('',#10538,#2456);
#1946=LINE('',#10540,#2457);
#1947=LINE('',#10541,#2458);
#1948=LINE('',#10544,#2459);
#1949=LINE('',#10546,#2460);
#1950=LINE('',#10547,#2461);
#1951=LINE('',#10549,#2462);
#1952=LINE('',#10550,#2463);
#1953=LINE('',#10562,#2464);
#1954=LINE('',#10566,#2465);
#1955=LINE('',#10570,#2466);
#1956=LINE('',#10577,#2467);
#1957=LINE('',#10579,#2468);
#1958=LINE('',#10586,#2469);
#1959=LINE('',#10594,#2470);
#1960=LINE('',#10615,#2471);
#1961=LINE('',#10670,#2472);
#1962=LINE('',#10675,#2473);
#1963=LINE('',#10681,#2474);
#1964=LINE('',#10689,#2475);
#1965=LINE('',#10710,#2476);
#1966=LINE('',#10765,#2477);
#1967=LINE('',#10770,#2478);
#1968=LINE('',#10776,#2479);
#1969=LINE('',#10785,#2480);
#1970=LINE('',#10791,#2481);
#1971=LINE('',#10800,#2482);
#1972=LINE('',#10806,#2483);
#1973=LINE('',#10814,#2484);
#1974=LINE('',#10835,#2485);
#1975=LINE('',#10890,#2486);
#1976=LINE('',#10895,#2487);
#1977=LINE('',#10901,#2488);
#1978=LINE('',#10910,#2489);
#1979=LINE('',#10916,#2490);
#1980=LINE('',#10924,#2491);
#1981=LINE('',#10945,#2492);
#1982=LINE('',#11000,#2493);
#1983=LINE('',#11005,#2494);
#1984=LINE('',#11011,#2495);
#1985=LINE('',#11019,#2496);
#1986=LINE('',#11040,#2497);
#1987=LINE('',#11095,#2498);
#1988=LINE('',#11100,#2499);
#1989=LINE('',#11108,#2500);
#1990=LINE('',#11112,#2501);
#1991=LINE('',#11114,#2502);
#1992=LINE('',#11116,#2503);
#1993=LINE('',#11117,#2504);
#1994=LINE('',#11120,#2505);
#1995=LINE('',#11122,#2506);
#1996=LINE('',#11123,#2507);
#1997=LINE('',#11126,#2508);
#1998=LINE('',#11128,#2509);
#1999=LINE('',#11129,#2510);
#2000=LINE('',#11132,#2511);
#2001=LINE('',#11134,#2512);
#2002=LINE('',#11135,#2513);
#2003=LINE('',#11138,#2514);
#2004=LINE('',#11140,#2515);
#2005=LINE('',#11141,#2516);
#2006=LINE('',#11144,#2517);
#2007=LINE('',#11146,#2518);
#2008=LINE('',#11147,#2519);
#2009=LINE('',#11150,#2520);
#2010=LINE('',#11152,#2521);
#2011=LINE('',#11153,#2522);
#2012=LINE('',#11156,#2523);
#2013=LINE('',#11158,#2524);
#2014=LINE('',#11159,#2525);
#2015=LINE('',#11162,#2526);
#2016=LINE('',#11164,#2527);
#2017=LINE('',#11165,#2528);
#2018=LINE('',#11168,#2529);
#2019=LINE('',#11170,#2530);
#2020=LINE('',#11171,#2531);
#2021=LINE('',#11174,#2532);
#2022=LINE('',#11176,#2533);
#2023=LINE('',#11177,#2534);
#2024=LINE('',#11180,#2535);
#2025=LINE('',#11182,#2536);
#2026=LINE('',#11183,#2537);
#2027=LINE('',#11186,#2538);
#2028=LINE('',#11188,#2539);
#2029=LINE('',#11189,#2540);
#2030=LINE('',#11192,#2541);
#2031=LINE('',#11194,#2542);
#2032=LINE('',#11195,#2543);
#2033=LINE('',#11198,#2544);
#2034=LINE('',#11200,#2545);
#2035=LINE('',#11201,#2546);
#2036=LINE('',#11204,#2547);
#2037=LINE('',#11206,#2548);
#2038=LINE('',#11207,#2549);
#2039=LINE('',#11210,#2550);
#2040=LINE('',#11212,#2551);
#2041=LINE('',#11213,#2552);
#2042=LINE('',#11216,#2553);
#2043=LINE('',#11218,#2554);
#2044=LINE('',#11219,#2555);
#2045=LINE('',#11222,#2556);
#2046=LINE('',#11224,#2557);
#2047=LINE('',#11225,#2558);
#2048=LINE('',#11228,#2559);
#2049=LINE('',#11230,#2560);
#2050=LINE('',#11231,#2561);
#2051=LINE('',#11234,#2562);
#2052=LINE('',#11236,#2563);
#2053=LINE('',#11237,#2564);
#2054=LINE('',#11240,#2565);
#2055=LINE('',#11242,#2566);
#2056=LINE('',#11243,#2567);
#2057=LINE('',#11246,#2568);
#2058=LINE('',#11248,#2569);
#2059=LINE('',#11249,#2570);
#2060=LINE('',#11252,#2571);
#2061=LINE('',#11254,#2572);
#2062=LINE('',#11255,#2573);
#2063=LINE('',#11258,#2574);
#2064=LINE('',#11260,#2575);
#2065=LINE('',#11261,#2576);
#2066=LINE('',#11264,#2577);
#2067=LINE('',#11266,#2578);
#2068=LINE('',#11267,#2579);
#2069=LINE('',#11270,#2580);
#2070=LINE('',#11272,#2581);
#2071=LINE('',#11273,#2582);
#2072=LINE('',#11276,#2583);
#2073=LINE('',#11278,#2584);
#2074=LINE('',#11279,#2585);
#2075=LINE('',#11282,#2586);
#2076=LINE('',#11284,#2587);
#2077=LINE('',#11285,#2588);
#2078=LINE('',#11288,#2589);
#2079=LINE('',#11290,#2590);
#2080=LINE('',#11291,#2591);
#2081=LINE('',#11294,#2592);
#2082=LINE('',#11296,#2593);
#2083=LINE('',#11297,#2594);
#2084=LINE('',#11300,#2595);
#2085=LINE('',#11302,#2596);
#2086=LINE('',#11303,#2597);
#2087=LINE('',#11306,#2598);
#2088=LINE('',#11308,#2599);
#2089=LINE('',#11309,#2600);
#2090=LINE('',#11312,#2601);
#2091=LINE('',#11314,#2602);
#2092=LINE('',#11315,#2603);
#2093=LINE('',#11318,#2604);
#2094=LINE('',#11320,#2605);
#2095=LINE('',#11321,#2606);
#2096=LINE('',#11324,#2607);
#2097=LINE('',#11326,#2608);
#2098=LINE('',#11327,#2609);
#2099=LINE('',#11330,#2610);
#2100=LINE('',#11332,#2611);
#2101=LINE('',#11333,#2612);
#2102=LINE('',#11336,#2613);
#2103=LINE('',#11338,#2614);
#2104=LINE('',#11339,#2615);
#2105=LINE('',#11342,#2616);
#2106=LINE('',#11344,#2617);
#2107=LINE('',#11345,#2618);
#2108=LINE('',#11348,#2619);
#2109=LINE('',#11350,#2620);
#2110=LINE('',#11351,#2621);
#2111=LINE('',#11354,#2622);
#2112=LINE('',#11356,#2623);
#2113=LINE('',#11357,#2624);
#2114=LINE('',#11360,#2625);
#2115=LINE('',#11362,#2626);
#2116=LINE('',#11363,#2627);
#2117=LINE('',#11366,#2628);
#2118=LINE('',#11368,#2629);
#2119=LINE('',#11369,#2630);
#2120=LINE('',#11372,#2631);
#2121=LINE('',#11374,#2632);
#2122=LINE('',#11375,#2633);
#2123=LINE('',#11378,#2634);
#2124=LINE('',#11380,#2635);
#2125=LINE('',#11381,#2636);
#2126=LINE('',#11384,#2637);
#2127=LINE('',#11386,#2638);
#2128=LINE('',#11387,#2639);
#2129=LINE('',#11390,#2640);
#2130=LINE('',#11392,#2641);
#2131=LINE('',#11393,#2642);
#2132=LINE('',#11395,#2643);
#2133=LINE('',#11396,#2644);
#2134=LINE('',#11404,#2645);
#2135=LINE('',#11409,#2646);
#2136=LINE('',#11430,#2647);
#2137=LINE('',#11450,#2648);
#2138=LINE('',#11456,#2649);
#2139=LINE('',#11458,#2650);
#2140=LINE('',#11460,#2651);
#2141=LINE('',#11466,#2652);
#2142=LINE('',#11468,#2653);
#2143=LINE('',#11469,#2654);
#2144=LINE('',#11474,#2655);
#2145=LINE('',#11475,#2656);
#2146=LINE('',#11477,#2657);
#2147=LINE('',#11478,#2658);
#2148=LINE('',#11483,#2659);
#2149=LINE('',#11487,#2660);
#2150=LINE('',#11494,#2661);
#2151=LINE('',#11501,#2662);
#2152=LINE('',#11509,#2663);
#2153=LINE('',#11511,#2664);
#2154=LINE('',#11513,#2665);
#2155=LINE('',#11514,#2666);
#2156=LINE('',#11517,#2667);
#2157=LINE('',#11519,#2668);
#2158=LINE('',#11520,#2669);
#2159=LINE('',#11523,#2670);
#2160=LINE('',#11525,#2671);
#2161=LINE('',#11526,#2672);
#2162=LINE('',#11529,#2673);
#2163=LINE('',#11531,#2674);
#2164=LINE('',#11532,#2675);
#2165=LINE('',#11535,#2676);
#2166=LINE('',#11537,#2677);
#2167=LINE('',#11538,#2678);
#2168=LINE('',#11540,#2679);
#2169=LINE('',#11541,#2680);
#2170=LINE('',#11549,#2681);
#2171=LINE('',#11553,#2682);
#2172=LINE('',#11557,#2683);
#2173=LINE('',#11566,#2684);
#2174=LINE('',#11570,#2685);
#2175=LINE('',#11574,#2686);
#2176=LINE('',#11581,#2687);
#2177=LINE('',#11585,#2688);
#2178=LINE('',#11589,#2689);
#2179=LINE('',#11594,#2690);
#2180=LINE('',#11596,#2691);
#2181=LINE('',#11598,#2692);
#2182=LINE('',#11599,#2693);
#2183=LINE('',#11602,#2694);
#2184=LINE('',#11604,#2695);
#2185=LINE('',#11605,#2696);
#2186=LINE('',#11608,#2697);
#2187=LINE('',#11610,#2698);
#2188=LINE('',#11611,#2699);
#2189=LINE('',#11614,#2700);
#2190=LINE('',#11616,#2701);
#2191=LINE('',#11617,#2702);
#2192=LINE('',#11620,#2703);
#2193=LINE('',#11622,#2704);
#2194=LINE('',#11623,#2705);
#2195=LINE('',#11625,#2706);
#2196=LINE('',#11626,#2707);
#2197=LINE('',#11690,#2708);
#2198=LINE('',#11695,#2709);
#2199=LINE('',#11699,#2710);
#2200=LINE('',#11703,#2711);
#2201=LINE('',#11705,#2712);
#2202=LINE('',#11706,#2713);
#2203=LINE('',#11709,#2714);
#2204=LINE('',#11710,#2715);
#2205=LINE('',#11713,#2716);
#2206=LINE('',#11714,#2717);
#2207=LINE('',#11716,#2718);
#2208=VECTOR('',#7368,0.210000000000001);
#2209=VECTOR('',#7375,0.21);
#2210=VECTOR('',#7382,0.21);
#2211=VECTOR('',#7389,0.21);
#2212=VECTOR('',#7396,0.21);
#2213=VECTOR('',#7403,0.21);
#2214=VECTOR('',#7410,0.21);
#2215=VECTOR('',#7417,0.21);
#2216=VECTOR('',#7424,0.21);
#2217=VECTOR('',#7431,0.21);
#2218=VECTOR('',#7436,1.);
#2219=VECTOR('',#7437,1.);
#2220=VECTOR('',#7438,1.);
#2221=VECTOR('',#7439,1.);
#2222=VECTOR('',#7442,1.);
#2223=VECTOR('',#7443,1.);
#2224=VECTOR('',#7444,1.);
#2225=VECTOR('',#7447,1.);
#2226=VECTOR('',#7448,1.);
#2227=VECTOR('',#7449,1.);
#2228=VECTOR('',#7452,1.);
#2229=VECTOR('',#7453,1.);
#2230=VECTOR('',#7462,1.);
#2231=VECTOR('',#7463,1.);
#2232=VECTOR('',#7464,1.);
#2233=VECTOR('',#7465,1.);
#2234=VECTOR('',#7468,1.);
#2235=VECTOR('',#7469,1.);
#2236=VECTOR('',#7470,1.);
#2237=VECTOR('',#7473,1.);
#2238=VECTOR('',#7474,1.);
#2239=VECTOR('',#7475,1.);
#2240=VECTOR('',#7478,1.);
#2241=VECTOR('',#7479,1.);
#2242=VECTOR('',#7488,1.);
#2243=VECTOR('',#7489,1.);
#2244=VECTOR('',#7490,1.);
#2245=VECTOR('',#7491,1.);
#2246=VECTOR('',#7494,1.);
#2247=VECTOR('',#7495,1.);
#2248=VECTOR('',#7496,1.);
#2249=VECTOR('',#7499,1.);
#2250=VECTOR('',#7500,1.);
#2251=VECTOR('',#7501,1.);
#2252=VECTOR('',#7504,1.);
#2253=VECTOR('',#7505,1.);
#2254=VECTOR('',#7516,0.475);
#2255=VECTOR('',#7527,0.475);
#2256=VECTOR('',#7538,0.275);
#2257=VECTOR('',#7543,0.275);
#2258=VECTOR('',#7548,0.475);
#2259=VECTOR('',#7559,0.475);
#2260=VECTOR('',#7570,0.275);
#2261=VECTOR('',#7575,0.275);
#2262=VECTOR('',#7580,0.34);
#2263=VECTOR('',#7587,0.34);
#2264=VECTOR('',#7592,1.);
#2265=VECTOR('',#7593,1.);
#2266=VECTOR('',#7594,1.);
#2267=VECTOR('',#7595,1.);
#2268=VECTOR('',#7598,1.);
#2269=VECTOR('',#7599,1.);
#2270=VECTOR('',#7600,1.);
#2271=VECTOR('',#7603,1.);
#2272=VECTOR('',#7604,1.);
#2273=VECTOR('',#7605,1.);
#2274=VECTOR('',#7608,1.);
#2275=VECTOR('',#7609,1.);
#2276=VECTOR('',#7620,0.425);
#2277=VECTOR('',#7627,0.645);
#2278=VECTOR('',#7640,0.425);
#2279=VECTOR('',#7647,0.645);
#2280=VECTOR('',#7660,0.475);
#2281=VECTOR('',#7671,0.475);
#2282=VECTOR('',#7682,0.275);
#2283=VECTOR('',#7687,0.275);
#2284=VECTOR('',#7692,0.475);
#2285=VECTOR('',#7703,0.475);
#2286=VECTOR('',#7714,0.275);
#2287=VECTOR('',#7719,0.275);
#2288=VECTOR('',#7724,0.34);
#2289=VECTOR('',#7731,0.34);
#2290=VECTOR('',#7736,1.);
#2291=VECTOR('',#7737,1.);
#2292=VECTOR('',#7738,1.);
#2293=VECTOR('',#7739,1.);
#2294=VECTOR('',#7742,1.);
#2295=VECTOR('',#7743,1.);
#2296=VECTOR('',#7744,1.);
#2297=VECTOR('',#7747,1.);
#2298=VECTOR('',#7748,1.);
#2299=VECTOR('',#7749,1.);
#2300=VECTOR('',#7752,1.);
#2301=VECTOR('',#7753,1.);
#2302=VECTOR('',#7764,0.425);
#2303=VECTOR('',#7771,0.645);
#2304=VECTOR('',#7784,0.425);
#2305=VECTOR('',#7791,0.645);
#2306=VECTOR('',#7804,0.275);
#2307=VECTOR('',#7811,0.275);
#2308=VECTOR('',#7818,0.305);
#2309=VECTOR('',#7823,1.);
#2310=VECTOR('',#7824,1.);
#2311=VECTOR('',#7825,1.);
#2312=VECTOR('',#7826,1.);
#2313=VECTOR('',#7827,1.);
#2314=VECTOR('',#7828,1.);
#2315=VECTOR('',#7829,1.);
#2316=VECTOR('',#7830,1.);
#2317=VECTOR('',#7833,1.);
#2318=VECTOR('',#7834,1.);
#2319=VECTOR('',#7835,1.);
#2320=VECTOR('',#7838,1.);
#2321=VECTOR('',#7839,1.);
#2322=VECTOR('',#7840,1.);
#2323=VECTOR('',#7843,1.);
#2324=VECTOR('',#7846,1.);
#2325=VECTOR('',#7849,1.);
#2326=VECTOR('',#7850,1.);
#2327=VECTOR('',#7851,1.);
#2328=VECTOR('',#7854,1.);
#2329=VECTOR('',#7855,1.);
#2330=VECTOR('',#7858,1.);
#2331=VECTOR('',#7859,1.);
#2332=VECTOR('',#7862,1.);
#2333=VECTOR('',#7873,0.165);
#2334=VECTOR('',#7886,0.6);
#2335=VECTOR('',#7895,0.3);
#2336=VECTOR('',#7904,0.305);
#2337=VECTOR('',#7911,0.5);
#2338=VECTOR('',#7924,0.225);
#2339=VECTOR('',#7931,0.6);
#2340=VECTOR('',#7942,1.);
#2341=VECTOR('',#7943,1.);
#2342=VECTOR('',#7944,1.);
#2343=VECTOR('',#7945,1.);
#2344=VECTOR('',#7948,1.);
#2345=VECTOR('',#7949,1.);
#2346=VECTOR('',#7950,1.);
#2347=VECTOR('',#7953,1.);
#2348=VECTOR('',#7954,1.);
#2349=VECTOR('',#7955,1.);
#2350=VECTOR('',#7958,1.);
#2351=VECTOR('',#7959,1.);
#2352=VECTOR('',#7970,0.164999999999999);
#2353=VECTOR('',#7975,1.);
#2354=VECTOR('',#7976,1.);
#2355=VECTOR('',#7977,1.);
#2356=VECTOR('',#7978,1.);
#2357=VECTOR('',#7981,1.);
#2358=VECTOR('',#7982,1.);
#2359=VECTOR('',#7983,1.);
#2360=VECTOR('',#7986,1.);
#2361=VECTOR('',#7987,1.);
#2362=VECTOR('',#7988,1.);
#2363=VECTOR('',#7991,1.);
#2364=VECTOR('',#7992,1.);
#2365=VECTOR('',#8005,2.05);
#2366=VECTOR('',#8012,2.05);
#2367=VECTOR('',#8021,1.);
#2368=VECTOR('',#8022,1.);
#2369=VECTOR('',#8027,1.);
#2370=VECTOR('',#8030,1.);
#2371=VECTOR('',#8033,1.);
#2372=VECTOR('',#8036,1.);
#2373=VECTOR('',#8039,1.);
#2374=VECTOR('',#8040,1.);
#2375=VECTOR('',#8043,1.);
#2376=VECTOR('',#8044,1.);
#2377=VECTOR('',#8049,1.);
#2378=VECTOR('',#8050,1.);
#2379=VECTOR('',#8053,1.);
#2380=VECTOR('',#8054,1.);
#2381=VECTOR('',#8055,1.);
#2382=VECTOR('',#8056,1.);
#2383=VECTOR('',#8061,1.);
#2384=VECTOR('',#8062,1.);
#2385=VECTOR('',#8063,1.);
#2386=VECTOR('',#8064,1.);
#2387=VECTOR('',#8065,1.);
#2388=VECTOR('',#8066,1.);
#2389=VECTOR('',#8079,1.);
#2390=VECTOR('',#8080,1.);
#2391=VECTOR('',#8081,1.);
#2392=VECTOR('',#8082,1.);
#2393=VECTOR('',#8085,1.);
#2394=VECTOR('',#8086,1.);
#2395=VECTOR('',#8087,1.);
#2396=VECTOR('',#8090,1.);
#2397=VECTOR('',#8091,1.);
#2398=VECTOR('',#8092,1.);
#2399=VECTOR('',#8095,1.);
#2400=VECTOR('',#8096,1.);
#2401=VECTOR('',#8103,0.65);
#2402=VECTOR('',#8108,0.65);
#2403=VECTOR('',#8111,1.);
#2404=VECTOR('',#8112,1.);
#2405=VECTOR('',#8113,1.);
#2406=VECTOR('',#8116,1.);
#2407=VECTOR('',#8117,1.);
#2408=VECTOR('',#8120,1.);
#2409=VECTOR('',#8121,1.);
#2410=VECTOR('',#8124,1.);
#2411=VECTOR('',#8133,1.8);
#2412=VECTOR('',#8150,0.25);
#2413=VECTOR('',#8153,0.25);
#2414=VECTOR('',#8158,1.65);
#2415=VECTOR('',#8163,0.25);
#2416=VECTOR('',#8166,0.25);
#2417=VECTOR('',#8169,0.25);
#2418=VECTOR('',#8172,0.25);
#2419=VECTOR('',#8185,1.75);
#2420=VECTOR('',#8192,1.);
#2421=VECTOR('',#8203,0.42);
#2422=VECTOR('',#8210,0.8);
#2423=VECTOR('',#8221,1.);
#2424=VECTOR('',#8222,1.);
#2425=VECTOR('',#8223,1.);
#2426=VECTOR('',#8224,1.);
#2427=VECTOR('',#8227,1.);
#2428=VECTOR('',#8228,1.);
#2429=VECTOR('',#8229,1.);
#2430=VECTOR('',#8232,1.);
#2431=VECTOR('',#8233,1.);
#2432=VECTOR('',#8234,1.);
#2433=VECTOR('',#8237,1.);
#2434=VECTOR('',#8238,1.);
#2435=VECTOR('',#8239,1.);
#2436=VECTOR('',#8242,1.);
#2437=VECTOR('',#8243,1.);
#2438=VECTOR('',#8244,1.);
#2439=VECTOR('',#8247,1.);
#2440=VECTOR('',#8248,1.);
#2441=VECTOR('',#8265,0.625);
#2442=VECTOR('',#8270,0.65);
#2443=VECTOR('',#8275,0.635);
#2444=VECTOR('',#8284,0.41);
#2445=VECTOR('',#8287,0.4);
#2446=VECTOR('',#8292,1.);
#2447=VECTOR('',#8293,1.);
#2448=VECTOR('',#8294,1.);
#2449=VECTOR('',#8295,1.);
#2450=VECTOR('',#8298,1.);
#2451=VECTOR('',#8299,1.);
#2452=VECTOR('',#8300,1.);
#2453=VECTOR('',#8303,1.);
#2454=VECTOR('',#8304,1.);
#2455=VECTOR('',#8305,1.);
#2456=VECTOR('',#8308,1.);
#2457=VECTOR('',#8309,1.);
#2458=VECTOR('',#8310,1.);
#2459=VECTOR('',#8313,1.);
#2460=VECTOR('',#8314,1.);
#2461=VECTOR('',#8315,1.);
#2462=VECTOR('',#8318,1.);
#2463=VECTOR('',#8319,1.);
#2464=VECTOR('',#8336,0.325);
#2465=VECTOR('',#8341,0.35);
#2466=VECTOR('',#8346,0.335);
#2467=VECTOR('',#8355,0.21);
#2468=VECTOR('',#8358,0.2);
#2469=VECTOR('',#8367,1.);
#2470=VECTOR('',#8378,1.);
#2471=VECTOR('',#8385,0.21);
#2472=VECTOR('',#8390,1.);
#2473=VECTOR('',#8395,1.005);
#2474=VECTOR('',#8402,1.5);
#2475=VECTOR('',#8413,1.);
#2476=VECTOR('',#8420,0.21);
#2477=VECTOR('',#8425,1.);
#2478=VECTOR('',#8430,1.005);
#2479=VECTOR('',#8437,1.5);
#2480=VECTOR('',#8450,3.6);
#2481=VECTOR('',#8457,4.);
#2482=VECTOR('',#8470,1.005);
#2483=VECTOR('',#8477,4.5);
#2484=VECTOR('',#8488,1.);
#2485=VECTOR('',#8495,0.21);
#2486=VECTOR('',#8500,1.);
#2487=VECTOR('',#8505,1.005);
#2488=VECTOR('',#8512,1.6);
#2489=VECTOR('',#8525,1.005);
#2490=VECTOR('',#8532,4.5);
#2491=VECTOR('',#8543,1.);
#2492=VECTOR('',#8550,0.21);
#2493=VECTOR('',#8555,1.);
#2494=VECTOR('',#8560,1.005);
#2495=VECTOR('',#8567,1.6);
#2496=VECTOR('',#8578,1.);
#2497=VECTOR('',#8585,0.21);
#2498=VECTOR('',#8590,1.);
#2499=VECTOR('',#8595,1.6);
#2500=VECTOR('',#8606,1.005);
#2501=VECTOR('',#8609,1.);
#2502=VECTOR('',#8610,1.);
#2503=VECTOR('',#8611,1.);
#2504=VECTOR('',#8612,1.);
#2505=VECTOR('',#8615,1.);
#2506=VECTOR('',#8616,1.);
#2507=VECTOR('',#8617,1.);
#2508=VECTOR('',#8620,1.);
#2509=VECTOR('',#8621,1.);
#2510=VECTOR('',#8622,1.);
#2511=VECTOR('',#8625,1.);
#2512=VECTOR('',#8626,1.);
#2513=VECTOR('',#8627,1.);
#2514=VECTOR('',#8630,1.);
#2515=VECTOR('',#8631,1.);
#2516=VECTOR('',#8632,1.);
#2517=VECTOR('',#8635,1.);
#2518=VECTOR('',#8636,1.);
#2519=VECTOR('',#8637,1.);
#2520=VECTOR('',#8640,1.);
#2521=VECTOR('',#8641,1.);
#2522=VECTOR('',#8642,1.);
#2523=VECTOR('',#8645,1.);
#2524=VECTOR('',#8646,1.);
#2525=VECTOR('',#8647,1.);
#2526=VECTOR('',#8650,1.);
#2527=VECTOR('',#8651,1.);
#2528=VECTOR('',#8652,1.);
#2529=VECTOR('',#8655,1.);
#2530=VECTOR('',#8656,1.);
#2531=VECTOR('',#8657,1.);
#2532=VECTOR('',#8660,1.);
#2533=VECTOR('',#8661,1.);
#2534=VECTOR('',#8662,1.);
#2535=VECTOR('',#8665,1.);
#2536=VECTOR('',#8666,1.);
#2537=VECTOR('',#8667,1.);
#2538=VECTOR('',#8670,1.);
#2539=VECTOR('',#8671,1.);
#2540=VECTOR('',#8672,1.);
#2541=VECTOR('',#8675,1.);
#2542=VECTOR('',#8676,1.);
#2543=VECTOR('',#8677,1.);
#2544=VECTOR('',#8680,1.);
#2545=VECTOR('',#8681,1.);
#2546=VECTOR('',#8682,1.);
#2547=VECTOR('',#8685,1.);
#2548=VECTOR('',#8686,1.);
#2549=VECTOR('',#8687,1.);
#2550=VECTOR('',#8690,1.);
#2551=VECTOR('',#8691,1.);
#2552=VECTOR('',#8692,1.);
#2553=VECTOR('',#8695,1.);
#2554=VECTOR('',#8696,1.);
#2555=VECTOR('',#8697,1.);
#2556=VECTOR('',#8700,1.);
#2557=VECTOR('',#8701,1.);
#2558=VECTOR('',#8702,1.);
#2559=VECTOR('',#8705,1.);
#2560=VECTOR('',#8706,1.);
#2561=VECTOR('',#8707,1.);
#2562=VECTOR('',#8710,1.);
#2563=VECTOR('',#8711,1.);
#2564=VECTOR('',#8712,1.);
#2565=VECTOR('',#8715,1.);
#2566=VECTOR('',#8716,1.);
#2567=VECTOR('',#8717,1.);
#2568=VECTOR('',#8720,1.);
#2569=VECTOR('',#8721,1.);
#2570=VECTOR('',#8722,1.);
#2571=VECTOR('',#8725,1.);
#2572=VECTOR('',#8726,1.);
#2573=VECTOR('',#8727,1.);
#2574=VECTOR('',#8730,1.);
#2575=VECTOR('',#8731,1.);
#2576=VECTOR('',#8732,1.);
#2577=VECTOR('',#8735,1.);
#2578=VECTOR('',#8736,1.);
#2579=VECTOR('',#8737,1.);
#2580=VECTOR('',#8740,1.);
#2581=VECTOR('',#8741,1.);
#2582=VECTOR('',#8742,1.);
#2583=VECTOR('',#8745,1.);
#2584=VECTOR('',#8746,1.);
#2585=VECTOR('',#8747,1.);
#2586=VECTOR('',#8750,1.);
#2587=VECTOR('',#8751,1.);
#2588=VECTOR('',#8752,1.);
#2589=VECTOR('',#8755,1.);
#2590=VECTOR('',#8756,1.);
#2591=VECTOR('',#8757,1.);
#2592=VECTOR('',#8760,1.);
#2593=VECTOR('',#8761,1.);
#2594=VECTOR('',#8762,1.);
#2595=VECTOR('',#8765,1.);
#2596=VECTOR('',#8766,1.);
#2597=VECTOR('',#8767,1.);
#2598=VECTOR('',#8770,1.);
#2599=VECTOR('',#8771,1.);
#2600=VECTOR('',#8772,1.);
#2601=VECTOR('',#8775,1.);
#2602=VECTOR('',#8776,1.);
#2603=VECTOR('',#8777,1.);
#2604=VECTOR('',#8780,1.);
#2605=VECTOR('',#8781,1.);
#2606=VECTOR('',#8782,1.);
#2607=VECTOR('',#8785,1.);
#2608=VECTOR('',#8786,1.);
#2609=VECTOR('',#8787,1.);
#2610=VECTOR('',#8790,1.);
#2611=VECTOR('',#8791,1.);
#2612=VECTOR('',#8792,1.);
#2613=VECTOR('',#8795,1.);
#2614=VECTOR('',#8796,1.);
#2615=VECTOR('',#8797,1.);
#2616=VECTOR('',#8800,1.);
#2617=VECTOR('',#8801,1.);
#2618=VECTOR('',#8802,1.);
#2619=VECTOR('',#8805,1.);
#2620=VECTOR('',#8806,1.);
#2621=VECTOR('',#8807,1.);
#2622=VECTOR('',#8810,1.);
#2623=VECTOR('',#8811,1.);
#2624=VECTOR('',#8812,1.);
#2625=VECTOR('',#8815,1.);
#2626=VECTOR('',#8816,1.);
#2627=VECTOR('',#8817,1.);
#2628=VECTOR('',#8820,1.);
#2629=VECTOR('',#8821,1.);
#2630=VECTOR('',#8822,1.);
#2631=VECTOR('',#8825,1.);
#2632=VECTOR('',#8826,1.);
#2633=VECTOR('',#8827,1.);
#2634=VECTOR('',#8830,1.);
#2635=VECTOR('',#8831,1.);
#2636=VECTOR('',#8832,1.);
#2637=VECTOR('',#8835,1.);
#2638=VECTOR('',#8836,1.);
#2639=VECTOR('',#8837,1.);
#2640=VECTOR('',#8840,1.);
#2641=VECTOR('',#8841,1.);
#2642=VECTOR('',#8842,1.);
#2643=VECTOR('',#8845,1.);
#2644=VECTOR('',#8846,1.);
#2645=VECTOR('',#8857,0.275);
#2646=VECTOR('',#8862,1.);
#2647=VECTOR('',#8869,0.21);
#2648=VECTOR('',#8878,1.);
#2649=VECTOR('',#8883,1.);
#2650=VECTOR('',#8884,1.);
#2651=VECTOR('',#8885,1.);
#2652=VECTOR('',#8892,1.);
#2653=VECTOR('',#8893,1.);
#2654=VECTOR('',#8894,1.);
#2655=VECTOR('',#8899,1.);
#2656=VECTOR('',#8900,1.);
#2657=VECTOR('',#8903,1.);
#2658=VECTOR('',#8904,1.);
#2659=VECTOR('',#8911,1.6);
#2660=VECTOR('',#8916,1.005);
#2661=VECTOR('',#8925,0.21);
#2662=VECTOR('',#8934,0.7);
#2663=VECTOR('',#8945,1.);
#2664=VECTOR('',#8946,1.);
#2665=VECTOR('',#8947,1.);
#2666=VECTOR('',#8948,1.);
#2667=VECTOR('',#8951,1.);
#2668=VECTOR('',#8952,1.);
#2669=VECTOR('',#8953,1.);
#2670=VECTOR('',#8956,1.);
#2671=VECTOR('',#8957,1.);
#2672=VECTOR('',#8958,1.);
#2673=VECTOR('',#8961,1.);
#2674=VECTOR('',#8962,1.);
#2675=VECTOR('',#8963,1.);
#2676=VECTOR('',#8966,1.);
#2677=VECTOR('',#8967,1.);
#2678=VECTOR('',#8968,1.);
#2679=VECTOR('',#8971,1.);
#2680=VECTOR('',#8972,1.);
#2681=VECTOR('',#8983,0.235);
#2682=VECTOR('',#8988,0.25);
#2683=VECTOR('',#8993,0.2125);
#2684=VECTOR('',#9006,0.4);
#2685=VECTOR('',#9011,0.425);
#2686=VECTOR('',#9016,0.41);
#2687=VECTOR('',#9025,0.26);
#2688=VECTOR('',#9030,0.25);
#2689=VECTOR('',#9035,0.225);
#2690=VECTOR('',#9040,1.);
#2691=VECTOR('',#9041,1.);
#2692=VECTOR('',#9042,1.);
#2693=VECTOR('',#9043,1.);
#2694=VECTOR('',#9046,1.);
#2695=VECTOR('',#9047,1.);
#2696=VECTOR('',#9048,1.);
#2697=VECTOR('',#9051,1.);
#2698=VECTOR('',#9052,1.);
#2699=VECTOR('',#9053,1.);
#2700=VECTOR('',#9056,1.);
#2701=VECTOR('',#9057,1.);
#2702=VECTOR('',#9058,1.);
#2703=VECTOR('',#9061,1.);
#2704=VECTOR('',#9062,1.);
#2705=VECTOR('',#9063,1.);
#2706=VECTOR('',#9066,1.);
#2707=VECTOR('',#9067,1.);
#2708=VECTOR('',#9190,0.305);
#2709=VECTOR('',#9195,1.);
#2710=VECTOR('',#9198,1.);
#2711=VECTOR('',#9203,1.);
#2712=VECTOR('',#9204,1.);
#2713=VECTOR('',#9205,1.);
#2714=VECTOR('',#9208,1.);
#2715=VECTOR('',#9209,1.);
#2716=VECTOR('',#9212,1.);
#2717=VECTOR('',#9213,1.);
#2718=VECTOR('',#9216,1.);
#2719=CIRCLE('',#6683,0.210000000000001);
#2720=CIRCLE('',#6684,0.210000000000001);
#2721=CIRCLE('',#6686,0.21);
#2722=CIRCLE('',#6687,0.21);
#2723=CIRCLE('',#6689,0.21);
#2724=CIRCLE('',#6690,0.21);
#2725=CIRCLE('',#6692,0.21);
#2726=CIRCLE('',#6693,0.21);
#2727=CIRCLE('',#6695,0.21);
#2728=CIRCLE('',#6696,0.21);
#2729=CIRCLE('',#6698,0.21);
#2730=CIRCLE('',#6699,0.21);
#2731=CIRCLE('',#6701,0.21);
#2732=CIRCLE('',#6702,0.21);
#2733=CIRCLE('',#6704,0.21);
#2734=CIRCLE('',#6705,0.21);
#2735=CIRCLE('',#6707,0.21);
#2736=CIRCLE('',#6708,0.21);
#2737=CIRCLE('',#6710,0.21);
#2738=CIRCLE('',#6711,0.21);
#2739=CIRCLE('',#6734,0.475);
#2740=CIRCLE('',#6735,0.475);
#2741=CIRCLE('',#6737,0.275);
#2742=CIRCLE('',#6739,0.475);
#2743=CIRCLE('',#6740,0.475);
#2744=CIRCLE('',#6742,0.275);
#2745=CIRCLE('',#6744,0.275);
#2746=CIRCLE('',#6746,0.275);
#2747=CIRCLE('',#6748,0.475);
#2748=CIRCLE('',#6749,0.475);
#2749=CIRCLE('',#6751,0.275);
#2750=CIRCLE('',#6753,0.475);
#2751=CIRCLE('',#6754,0.475);
#2752=CIRCLE('',#6756,0.275);
#2753=CIRCLE('',#6758,0.275);
#2754=CIRCLE('',#6760,0.275);
#2755=CIRCLE('',#6762,0.34);
#2756=CIRCLE('',#6763,0.34);
#2757=CIRCLE('',#6765,0.34);
#2758=CIRCLE('',#6766,0.34);
#2759=CIRCLE('',#6775,0.425);
#2760=CIRCLE('',#6776,0.425);
#2761=CIRCLE('',#6778,0.645);
#2762=CIRCLE('',#6779,0.645);
#2763=CIRCLE('',#6784,0.425);
#2764=CIRCLE('',#6785,0.425);
#2765=CIRCLE('',#6787,0.645);
#2766=CIRCLE('',#6788,0.645);
#2767=CIRCLE('',#6793,0.475);
#2768=CIRCLE('',#6794,0.475);
#2769=CIRCLE('',#6796,0.275);
#2770=CIRCLE('',#6798,0.475);
#2771=CIRCLE('',#6799,0.475);
#2772=CIRCLE('',#6801,0.275);
#2773=CIRCLE('',#6803,0.275);
#2774=CIRCLE('',#6805,0.275);
#2775=CIRCLE('',#6807,0.475);
#2776=CIRCLE('',#6808,0.475);
#2777=CIRCLE('',#6810,0.275);
#2778=CIRCLE('',#6812,0.475);
#2779=CIRCLE('',#6813,0.475);
#2780=CIRCLE('',#6815,0.275);
#2781=CIRCLE('',#6817,0.275);
#2782=CIRCLE('',#6819,0.275);
#2783=CIRCLE('',#6821,0.34);
#2784=CIRCLE('',#6822,0.34);
#2785=CIRCLE('',#6824,0.34);
#2786=CIRCLE('',#6825,0.34);
#2787=CIRCLE('',#6834,0.425);
#2788=CIRCLE('',#6835,0.425);
#2789=CIRCLE('',#6837,0.645);
#2790=CIRCLE('',#6838,0.645);
#2791=CIRCLE('',#6843,0.425);
#2792=CIRCLE('',#6844,0.425);
#2793=CIRCLE('',#6846,0.645);
#2794=CIRCLE('',#6847,0.645);
#2795=CIRCLE('',#6852,0.275);
#2796=CIRCLE('',#6853,0.275);
#2797=CIRCLE('',#6855,0.275);
#2798=CIRCLE('',#6856,0.275);
#2799=CIRCLE('',#6858,0.305);
#2800=CIRCLE('',#6859,0.305);
#2801=CIRCLE('',#6873,0.165);
#2802=CIRCLE('',#6874,0.165);
#2803=CIRCLE('',#6877,0.6);
#2804=CIRCLE('',#6878,0.3);
#2805=CIRCLE('',#6880,0.6);
#2806=CIRCLE('',#6883,0.3);
#2807=CIRCLE('',#6887,0.305);
#2808=CIRCLE('',#6888,0.305);
#2809=CIRCLE('',#6890,0.5);
#2810=CIRCLE('',#6891,0.5);
#2811=CIRCLE('',#6896,0.225);
#2812=CIRCLE('',#6897,0.225);
#2813=CIRCLE('',#6899,0.6);
#2814=CIRCLE('',#6900,0.6);
#2815=CIRCLE('',#6912,0.164999999999999);
#2816=CIRCLE('',#6913,0.164999999999999);
#2817=CIRCLE('',#6923,2.05);
#2818=CIRCLE('',#6924,2.05);
#2819=CIRCLE('',#6926,2.05);
#2820=CIRCLE('',#6927,2.05);
#2821=CIRCLE('',#6929,2.35);
#2822=CIRCLE('',#6931,2.8);
#2823=CIRCLE('',#6933,2.8);
#2824=CIRCLE('',#6935,2.8);
#2825=CIRCLE('',#6938,2.8);
#2826=CIRCLE('',#6941,0.65);
#2827=CIRCLE('',#6942,0.65);
#2828=CIRCLE('',#6944,2.8);
#2829=CIRCLE('',#6945,2.8);
#2830=CIRCLE('',#6954,0.65);
#2831=CIRCLE('',#6956,0.65);
#2832=CIRCLE('',#6964,1.8);
#2833=CIRCLE('',#6965,1.8);
#2834=CIRCLE('',#6967,2.19089023002066);
#2835=CIRCLE('',#6969,2.35);
#2836=CIRCLE('',#6970,2.19089023002066);
#2837=CIRCLE('',#6975,1.65);
#2838=CIRCLE('',#6976,1.65);
#2839=CIRCLE('',#6982,1.);
#2840=CIRCLE('',#6984,1.75);
#2841=CIRCLE('',#6986,1.75);
#2842=CIRCLE('',#6988,1.);
#2843=CIRCLE('',#6994,0.42);
#2844=CIRCLE('',#6995,0.42);
#2845=CIRCLE('',#6997,0.8);
#2846=CIRCLE('',#6998,0.8);
#2847=CIRCLE('',#7011,0.3933);
#2848=CIRCLE('',#7013,0.6);
#2849=CIRCLE('',#7015,0.65);
#2850=CIRCLE('',#7017,0.65);
#2851=CIRCLE('',#7019,0.62);
#2852=CIRCLE('',#7021,0.42);
#2853=CIRCLE('',#7023,0.3933);
#2854=CIRCLE('',#7035,0.1954);
#2855=CIRCLE('',#7037,0.3);
#2856=CIRCLE('',#7039,0.35);
#2857=CIRCLE('',#7041,0.35);
#2858=CIRCLE('',#7043,0.32);
#2859=CIRCLE('',#7045,0.22);
#2860=CIRCLE('',#7047,0.1954);
#2861=CIRCLE('',#7052,1.);
#2862=CIRCLE('',#7053,1.);
#2863=CIRCLE('',#7058,0.21);
#2864=CIRCLE('',#7060,0.21);
#2865=CIRCLE('',#7061,0.21);
#2866=CIRCLE('',#7064,1.005);
#2867=CIRCLE('',#7065,1.005);
#2868=CIRCLE('',#7067,1.5);
#2869=CIRCLE('',#7068,1.5);
#2870=CIRCLE('',#7073,0.21);
#2871=CIRCLE('',#7075,0.21);
#2872=CIRCLE('',#7076,0.21);
#2873=CIRCLE('',#7079,1.005);
#2874=CIRCLE('',#7080,1.005);
#2875=CIRCLE('',#7082,1.5);
#2876=CIRCLE('',#7083,1.5);
#2877=CIRCLE('',#7088,3.6);
#2878=CIRCLE('',#7089,3.6);
#2879=CIRCLE('',#7091,4.);
#2880=CIRCLE('',#7092,4.);
#2881=CIRCLE('',#7097,1.005);
#2882=CIRCLE('',#7098,1.005);
#2883=CIRCLE('',#7100,4.5);
#2884=CIRCLE('',#7101,4.5);
#2885=CIRCLE('',#7106,0.21);
#2886=CIRCLE('',#7108,0.21);
#2887=CIRCLE('',#7109,0.21);
#2888=CIRCLE('',#7112,1.005);
#2889=CIRCLE('',#7113,1.005);
#2890=CIRCLE('',#7115,1.6);
#2891=CIRCLE('',#7116,1.6);
#2892=CIRCLE('',#7121,1.005);
#2893=CIRCLE('',#7122,1.005);
#2894=CIRCLE('',#7124,4.5);
#2895=CIRCLE('',#7125,4.5);
#2896=CIRCLE('',#7130,0.21);
#2897=CIRCLE('',#7132,0.21);
#2898=CIRCLE('',#7133,0.21);
#2899=CIRCLE('',#7136,1.005);
#2900=CIRCLE('',#7137,1.005);
#2901=CIRCLE('',#7139,1.6);
#2902=CIRCLE('',#7140,1.6);
#2903=CIRCLE('',#7145,0.21);
#2904=CIRCLE('',#7147,0.21);
#2905=CIRCLE('',#7148,0.21);
#2906=CIRCLE('',#7151,1.6);
#2907=CIRCLE('',#7152,1.6);
#2908=CIRCLE('',#7154,1.005);
#2909=CIRCLE('',#7156,1.005);
#2910=CIRCLE('',#7209,0.275);
#2911=CIRCLE('',#7210,0.275);
#2912=CIRCLE('',#7212,0.21);
#2913=CIRCLE('',#7214,0.21);
#2914=CIRCLE('',#7215,0.21);
#2915=CIRCLE('',#7216,0.21);
#2916=CIRCLE('',#7220,1.6);
#2917=CIRCLE('',#7221,1.6);
#2918=CIRCLE('',#7222,1.005);
#2919=CIRCLE('',#7225,1.6);
#2920=CIRCLE('',#7229,1.6);
#2921=CIRCLE('',#7231,1.005);
#2922=CIRCLE('',#7235,0.21);
#2923=CIRCLE('',#7236,0.21);
#2924=CIRCLE('',#7239,0.7);
#2925=CIRCLE('',#7240,0.7);
#2926=CIRCLE('',#7252,0.22);
#2927=CIRCLE('',#7254,0.24505);
#2928=CIRCLE('',#7256,0.24505);
#2929=CIRCLE('',#7258,0.175);
#2930=CIRCLE('',#7262,0.375);
#2931=CIRCLE('',#7264,0.425);
#2932=CIRCLE('',#7266,0.425);
#2933=CIRCLE('',#7268,0.395);
#2934=CIRCLE('',#7270,0.27);
#2935=CIRCLE('',#7272,0.24505);
#2936=CIRCLE('',#7274,0.24505);
#2937=CIRCLE('',#7276,0.2);
#2938=CIRCLE('',#7344,0.305);
#2939=CIRCLE('',#7345,0.305);
#2940=CIRCLE('',#7347,0.7);
#2941=CIRCLE('',#7348,0.7);
#2942=VERTEX_POINT('',#9231);
#2943=VERTEX_POINT('',#9233);
#2944=VERTEX_POINT('',#9237);
#2945=VERTEX_POINT('',#9239);
#2946=VERTEX_POINT('',#9243);
#2947=VERTEX_POINT('',#9245);
#2948=VERTEX_POINT('',#9249);
#2949=VERTEX_POINT('',#9251);
#2950=VERTEX_POINT('',#9255);
#2951=VERTEX_POINT('',#9257);
#2952=VERTEX_POINT('',#9261);
#2953=VERTEX_POINT('',#9263);
#2954=VERTEX_POINT('',#9267);
#2955=VERTEX_POINT('',#9269);
#2956=VERTEX_POINT('',#9273);
#2957=VERTEX_POINT('',#9275);
#2958=VERTEX_POINT('',#9279);
#2959=VERTEX_POINT('',#9281);
#2960=VERTEX_POINT('',#9285);
#2961=VERTEX_POINT('',#9287);
#2962=VERTEX_POINT('',#9291);
#2963=VERTEX_POINT('',#9292);
#2964=VERTEX_POINT('',#9294);
#2965=VERTEX_POINT('',#9296);
#2966=VERTEX_POINT('',#9300);
#2967=VERTEX_POINT('',#9302);
#2968=VERTEX_POINT('',#9306);
#2969=VERTEX_POINT('',#9308);
#2970=VERTEX_POINT('',#9318);
#2971=VERTEX_POINT('',#9319);
#2972=VERTEX_POINT('',#9321);
#2973=VERTEX_POINT('',#9323);
#2974=VERTEX_POINT('',#9327);
#2975=VERTEX_POINT('',#9329);
#2976=VERTEX_POINT('',#9333);
#2977=VERTEX_POINT('',#9335);
#2978=VERTEX_POINT('',#9345);
#2979=VERTEX_POINT('',#9346);
#2980=VERTEX_POINT('',#9348);
#2981=VERTEX_POINT('',#9350);
#2982=VERTEX_POINT('',#9354);
#2983=VERTEX_POINT('',#9356);
#2984=VERTEX_POINT('',#9360);
#2985=VERTEX_POINT('',#9362);
#2986=VERTEX_POINT('',#9372);
#2987=VERTEX_POINT('',#9374);
#2988=VERTEX_POINT('',#9378);
#2989=VERTEX_POINT('',#9381);
#2990=VERTEX_POINT('',#9383);
#2991=VERTEX_POINT('',#9387);
#2992=VERTEX_POINT('',#9390);
#2993=VERTEX_POINT('',#9394);
#2994=VERTEX_POINT('',#9398);
#2995=VERTEX_POINT('',#9400);
#2996=VERTEX_POINT('',#9404);
#2997=VERTEX_POINT('',#9407);
#2998=VERTEX_POINT('',#9409);
#2999=VERTEX_POINT('',#9413);
#3000=VERTEX_POINT('',#9416);
#3001=VERTEX_POINT('',#9420);
#3002=VERTEX_POINT('',#9424);
#3003=VERTEX_POINT('',#9426);
#3004=VERTEX_POINT('',#9430);
#3005=VERTEX_POINT('',#9432);
#3006=VERTEX_POINT('',#9436);
#3007=VERTEX_POINT('',#9437);
#3008=VERTEX_POINT('',#9439);
#3009=VERTEX_POINT('',#9441);
#3010=VERTEX_POINT('',#9445);
#3011=VERTEX_POINT('',#9447);
#3012=VERTEX_POINT('',#9451);
#3013=VERTEX_POINT('',#9453);
#3014=VERTEX_POINT('',#9463);
#3015=VERTEX_POINT('',#9465);
#3016=VERTEX_POINT('',#9469);
#3017=VERTEX_POINT('',#9471);
#3018=VERTEX_POINT('',#9478);
#3019=VERTEX_POINT('',#9480);
#3020=VERTEX_POINT('',#9484);
#3021=VERTEX_POINT('',#9486);
#3022=VERTEX_POINT('',#9493);
#3023=VERTEX_POINT('',#9495);
#3024=VERTEX_POINT('',#9499);
#3025=VERTEX_POINT('',#9502);
#3026=VERTEX_POINT('',#9504);
#3027=VERTEX_POINT('',#9508);
#3028=VERTEX_POINT('',#9511);
#3029=VERTEX_POINT('',#9515);
#3030=VERTEX_POINT('',#9519);
#3031=VERTEX_POINT('',#9521);
#3032=VERTEX_POINT('',#9525);
#3033=VERTEX_POINT('',#9528);
#3034=VERTEX_POINT('',#9530);
#3035=VERTEX_POINT('',#9534);
#3036=VERTEX_POINT('',#9537);
#3037=VERTEX_POINT('',#9541);
#3038=VERTEX_POINT('',#9545);
#3039=VERTEX_POINT('',#9547);
#3040=VERTEX_POINT('',#9551);
#3041=VERTEX_POINT('',#9553);
#3042=VERTEX_POINT('',#9557);
#3043=VERTEX_POINT('',#9558);
#3044=VERTEX_POINT('',#9560);
#3045=VERTEX_POINT('',#9562);
#3046=VERTEX_POINT('',#9566);
#3047=VERTEX_POINT('',#9568);
#3048=VERTEX_POINT('',#9572);
#3049=VERTEX_POINT('',#9574);
#3050=VERTEX_POINT('',#9584);
#3051=VERTEX_POINT('',#9586);
#3052=VERTEX_POINT('',#9590);
#3053=VERTEX_POINT('',#9592);
#3054=VERTEX_POINT('',#9599);
#3055=VERTEX_POINT('',#9601);
#3056=VERTEX_POINT('',#9605);
#3057=VERTEX_POINT('',#9607);
#3058=VERTEX_POINT('',#9614);
#3059=VERTEX_POINT('',#9616);
#3060=VERTEX_POINT('',#9620);
#3061=VERTEX_POINT('',#9622);
#3062=VERTEX_POINT('',#9626);
#3063=VERTEX_POINT('',#9628);
#3064=VERTEX_POINT('',#9632);
#3065=VERTEX_POINT('',#9633);
#3066=VERTEX_POINT('',#9635);
#3067=VERTEX_POINT('',#9637);
#3068=VERTEX_POINT('',#9640);
#3069=VERTEX_POINT('',#9641);
#3070=VERTEX_POINT('',#9643);
#3071=VERTEX_POINT('',#9645);
#3072=VERTEX_POINT('',#9649);
#3073=VERTEX_POINT('',#9651);
#3074=VERTEX_POINT('',#9655);
#3075=VERTEX_POINT('',#9657);
#3076=VERTEX_POINT('',#9665);
#3077=VERTEX_POINT('',#9667);
#3078=VERTEX_POINT('',#9671);
#3079=VERTEX_POINT('',#9675);
#3080=VERTEX_POINT('',#9684);
#3081=VERTEX_POINT('',#9686);
#3082=VERTEX_POINT('',#9691);
#3083=VERTEX_POINT('',#9693);
#3084=VERTEX_POINT('',#9696);
#3085=VERTEX_POINT('',#9701);
#3086=VERTEX_POINT('',#9707);
#3087=VERTEX_POINT('',#9709);
#3088=VERTEX_POINT('',#9713);
#3089=VERTEX_POINT('',#9715);
#3090=VERTEX_POINT('',#9722);
#3091=VERTEX_POINT('',#9724);
#3092=VERTEX_POINT('',#9728);
#3093=VERTEX_POINT('',#9730);
#3094=VERTEX_POINT('',#9737);
#3095=VERTEX_POINT('',#9738);
#3096=VERTEX_POINT('',#9740);
#3097=VERTEX_POINT('',#9742);
#3098=VERTEX_POINT('',#9746);
#3099=VERTEX_POINT('',#9748);
#3100=VERTEX_POINT('',#9752);
#3101=VERTEX_POINT('',#9754);
#3102=VERTEX_POINT('',#9764);
#3103=VERTEX_POINT('',#9766);
#3104=VERTEX_POINT('',#9770);
#3105=VERTEX_POINT('',#9771);
#3106=VERTEX_POINT('',#9773);
#3107=VERTEX_POINT('',#9775);
#3108=VERTEX_POINT('',#9779);
#3109=VERTEX_POINT('',#9781);
#3110=VERTEX_POINT('',#9785);
#3111=VERTEX_POINT('',#9787);
#3112=VERTEX_POINT('',#9798);
#3113=VERTEX_POINT('',#9800);
#3114=VERTEX_POINT('',#9804);
#3115=VERTEX_POINT('',#9806);
#3116=VERTEX_POINT('',#9810);
#3117=VERTEX_POINT('',#9811);
#3118=VERTEX_POINT('',#9814);
#3119=VERTEX_POINT('',#9815);
#3120=VERTEX_POINT('',#9817);
#3121=VERTEX_POINT('',#9821);
#3122=VERTEX_POINT('',#9822);
#3123=VERTEX_POINT('',#9824);
#3124=VERTEX_POINT('',#9828);
#3125=VERTEX_POINT('',#9829);
#3126=VERTEX_POINT('',#9831);
#3127=VERTEX_POINT('',#9838);
#3128=VERTEX_POINT('',#9839);
#3129=VERTEX_POINT('',#9841);
#3130=VERTEX_POINT('',#9848);
#3131=VERTEX_POINT('',#9849);
#3132=VERTEX_POINT('',#9851);
#3133=VERTEX_POINT('',#9853);
#3134=VERTEX_POINT('',#9856);
#3135=VERTEX_POINT('',#9858);
#3136=VERTEX_POINT('',#9860);
#3137=VERTEX_POINT('',#9862);
#3138=VERTEX_POINT('',#9865);
#3139=VERTEX_POINT('',#9867);
#3140=VERTEX_POINT('',#9876);
#3141=VERTEX_POINT('',#9877);
#3142=VERTEX_POINT('',#9879);
#3143=VERTEX_POINT('',#9881);
#3144=VERTEX_POINT('',#9885);
#3145=VERTEX_POINT('',#9887);
#3146=VERTEX_POINT('',#9891);
#3147=VERTEX_POINT('',#9893);
#3148=VERTEX_POINT('',#9901);
#3149=VERTEX_POINT('',#9905);
#3150=VERTEX_POINT('',#9909);
#3151=VERTEX_POINT('',#9910);
#3152=VERTEX_POINT('',#9915);
#3153=VERTEX_POINT('',#9919);
#3154=VERTEX_POINT('',#9927);
#3155=VERTEX_POINT('',#9929);
#3156=VERTEX_POINT('',#9933);
#3157=VERTEX_POINT('',#9936);
#3158=VERTEX_POINT('',#9937);
#3159=VERTEX_POINT('',#9939);
#3160=VERTEX_POINT('',#9943);
#3161=VERTEX_POINT('',#9944);
#3162=VERTEX_POINT('',#9955);
#3163=VERTEX_POINT('',#9984);
#3164=VERTEX_POINT('',#10021);
#3165=VERTEX_POINT('',#10056);
#3166=VERTEX_POINT('',#10058);
#3167=VERTEX_POINT('',#10069);
#3168=VERTEX_POINT('',#10099);
#3169=VERTEX_POINT('',#10101);
#3170=VERTEX_POINT('',#10104);
#3171=VERTEX_POINT('',#10105);
#3172=VERTEX_POINT('',#10124);
#3173=VERTEX_POINT('',#10145);
#3174=VERTEX_POINT('',#10146);
#3175=VERTEX_POINT('',#10165);
#3176=VERTEX_POINT('',#10186);
#3177=VERTEX_POINT('',#10187);
#3178=VERTEX_POINT('',#10206);
#3179=VERTEX_POINT('',#10227);
#3180=VERTEX_POINT('',#10228);
#3181=VERTEX_POINT('',#10247);
#3182=VERTEX_POINT('',#10269);
#3183=VERTEX_POINT('',#10306);
#3184=VERTEX_POINT('',#10343);
#3185=VERTEX_POINT('',#10380);
#3186=VERTEX_POINT('',#10417);
#3187=VERTEX_POINT('',#10420);
#3188=VERTEX_POINT('',#10423);
#3189=VERTEX_POINT('',#10427);
#3190=VERTEX_POINT('',#10435);
#3191=VERTEX_POINT('',#10437);
#3192=VERTEX_POINT('',#10441);
#3193=VERTEX_POINT('',#10443);
#3194=VERTEX_POINT('',#10450);
#3195=VERTEX_POINT('',#10451);
#3196=VERTEX_POINT('',#10453);
#3197=VERTEX_POINT('',#10455);
#3198=VERTEX_POINT('',#10459);
#3199=VERTEX_POINT('',#10461);
#3200=VERTEX_POINT('',#10465);
#3201=VERTEX_POINT('',#10467);
#3202=VERTEX_POINT('',#10471);
#3203=VERTEX_POINT('',#10473);
#3204=VERTEX_POINT('',#10477);
#3205=VERTEX_POINT('',#10479);
#3206=VERTEX_POINT('',#10488);
#3207=VERTEX_POINT('',#10491);
#3208=VERTEX_POINT('',#10494);
#3209=VERTEX_POINT('',#10498);
#3210=VERTEX_POINT('',#10502);
#3211=VERTEX_POINT('',#10506);
#3212=VERTEX_POINT('',#10509);
#3213=VERTEX_POINT('',#10516);
#3214=VERTEX_POINT('',#10517);
#3215=VERTEX_POINT('',#10519);
#3216=VERTEX_POINT('',#10521);
#3217=VERTEX_POINT('',#10525);
#3218=VERTEX_POINT('',#10527);
#3219=VERTEX_POINT('',#10531);
#3220=VERTEX_POINT('',#10533);
#3221=VERTEX_POINT('',#10537);
#3222=VERTEX_POINT('',#10539);
#3223=VERTEX_POINT('',#10543);
#3224=VERTEX_POINT('',#10545);
#3225=VERTEX_POINT('',#10554);
#3226=VERTEX_POINT('',#10557);
#3227=VERTEX_POINT('',#10560);
#3228=VERTEX_POINT('',#10564);
#3229=VERTEX_POINT('',#10568);
#3230=VERTEX_POINT('',#10572);
#3231=VERTEX_POINT('',#10575);
#3232=VERTEX_POINT('',#10583);
#3233=VERTEX_POINT('',#10585);
#3234=VERTEX_POINT('',#10592);
#3235=VERTEX_POINT('',#10593);
#3236=VERTEX_POINT('',#10597);
#3237=VERTEX_POINT('',#10612);
#3238=VERTEX_POINT('',#10614);
#3239=VERTEX_POINT('',#10616);
#3240=VERTEX_POINT('',#10653);
#3241=VERTEX_POINT('',#10672);
#3242=VERTEX_POINT('',#10674);
#3243=VERTEX_POINT('',#10678);
#3244=VERTEX_POINT('',#10680);
#3245=VERTEX_POINT('',#10687);
#3246=VERTEX_POINT('',#10688);
#3247=VERTEX_POINT('',#10692);
#3248=VERTEX_POINT('',#10707);
#3249=VERTEX_POINT('',#10709);
#3250=VERTEX_POINT('',#10711);
#3251=VERTEX_POINT('',#10748);
#3252=VERTEX_POINT('',#10767);
#3253=VERTEX_POINT('',#10769);
#3254=VERTEX_POINT('',#10773);
#3255=VERTEX_POINT('',#10775);
#3256=VERTEX_POINT('',#10782);
#3257=VERTEX_POINT('',#10784);
#3258=VERTEX_POINT('',#10788);
#3259=VERTEX_POINT('',#10790);
#3260=VERTEX_POINT('',#10797);
#3261=VERTEX_POINT('',#10799);
#3262=VERTEX_POINT('',#10803);
#3263=VERTEX_POINT('',#10805);
#3264=VERTEX_POINT('',#10812);
#3265=VERTEX_POINT('',#10813);
#3266=VERTEX_POINT('',#10817);
#3267=VERTEX_POINT('',#10832);
#3268=VERTEX_POINT('',#10834);
#3269=VERTEX_POINT('',#10836);
#3270=VERTEX_POINT('',#10873);
#3271=VERTEX_POINT('',#10892);
#3272=VERTEX_POINT('',#10894);
#3273=VERTEX_POINT('',#10898);
#3274=VERTEX_POINT('',#10900);
#3275=VERTEX_POINT('',#10907);
#3276=VERTEX_POINT('',#10909);
#3277=VERTEX_POINT('',#10913);
#3278=VERTEX_POINT('',#10915);
#3279=VERTEX_POINT('',#10922);
#3280=VERTEX_POINT('',#10923);
#3281=VERTEX_POINT('',#10927);
#3282=VERTEX_POINT('',#10942);
#3283=VERTEX_POINT('',#10944);
#3284=VERTEX_POINT('',#10946);
#3285=VERTEX_POINT('',#10983);
#3286=VERTEX_POINT('',#11002);
#3287=VERTEX_POINT('',#11004);
#3288=VERTEX_POINT('',#11008);
#3289=VERTEX_POINT('',#11010);
#3290=VERTEX_POINT('',#11017);
#3291=VERTEX_POINT('',#11018);
#3292=VERTEX_POINT('',#11022);
#3293=VERTEX_POINT('',#11037);
#3294=VERTEX_POINT('',#11039);
#3295=VERTEX_POINT('',#11041);
#3296=VERTEX_POINT('',#11078);
#3297=VERTEX_POINT('',#11097);
#3298=VERTEX_POINT('',#11099);
#3299=VERTEX_POINT('',#11103);
#3300=VERTEX_POINT('',#11106);
#3301=VERTEX_POINT('',#11110);
#3302=VERTEX_POINT('',#11111);
#3303=VERTEX_POINT('',#11113);
#3304=VERTEX_POINT('',#11115);
#3305=VERTEX_POINT('',#11119);
#3306=VERTEX_POINT('',#11121);
#3307=VERTEX_POINT('',#11125);
#3308=VERTEX_POINT('',#11127);
#3309=VERTEX_POINT('',#11131);
#3310=VERTEX_POINT('',#11133);
#3311=VERTEX_POINT('',#11137);
#3312=VERTEX_POINT('',#11139);
#3313=VERTEX_POINT('',#11143);
#3314=VERTEX_POINT('',#11145);
#3315=VERTEX_POINT('',#11149);
#3316=VERTEX_POINT('',#11151);
#3317=VERTEX_POINT('',#11155);
#3318=VERTEX_POINT('',#11157);
#3319=VERTEX_POINT('',#11161);
#3320=VERTEX_POINT('',#11163);
#3321=VERTEX_POINT('',#11167);
#3322=VERTEX_POINT('',#11169);
#3323=VERTEX_POINT('',#11173);
#3324=VERTEX_POINT('',#11175);
#3325=VERTEX_POINT('',#11179);
#3326=VERTEX_POINT('',#11181);
#3327=VERTEX_POINT('',#11185);
#3328=VERTEX_POINT('',#11187);
#3329=VERTEX_POINT('',#11191);
#3330=VERTEX_POINT('',#11193);
#3331=VERTEX_POINT('',#11197);
#3332=VERTEX_POINT('',#11199);
#3333=VERTEX_POINT('',#11203);
#3334=VERTEX_POINT('',#11205);
#3335=VERTEX_POINT('',#11209);
#3336=VERTEX_POINT('',#11211);
#3337=VERTEX_POINT('',#11215);
#3338=VERTEX_POINT('',#11217);
#3339=VERTEX_POINT('',#11221);
#3340=VERTEX_POINT('',#11223);
#3341=VERTEX_POINT('',#11227);
#3342=VERTEX_POINT('',#11229);
#3343=VERTEX_POINT('',#11233);
#3344=VERTEX_POINT('',#11235);
#3345=VERTEX_POINT('',#11239);
#3346=VERTEX_POINT('',#11241);
#3347=VERTEX_POINT('',#11245);
#3348=VERTEX_POINT('',#11247);
#3349=VERTEX_POINT('',#11251);
#3350=VERTEX_POINT('',#11253);
#3351=VERTEX_POINT('',#11257);
#3352=VERTEX_POINT('',#11259);
#3353=VERTEX_POINT('',#11263);
#3354=VERTEX_POINT('',#11265);
#3355=VERTEX_POINT('',#11269);
#3356=VERTEX_POINT('',#11271);
#3357=VERTEX_POINT('',#11275);
#3358=VERTEX_POINT('',#11277);
#3359=VERTEX_POINT('',#11281);
#3360=VERTEX_POINT('',#11283);
#3361=VERTEX_POINT('',#11287);
#3362=VERTEX_POINT('',#11289);
#3363=VERTEX_POINT('',#11293);
#3364=VERTEX_POINT('',#11295);
#3365=VERTEX_POINT('',#11299);
#3366=VERTEX_POINT('',#11301);
#3367=VERTEX_POINT('',#11305);
#3368=VERTEX_POINT('',#11307);
#3369=VERTEX_POINT('',#11311);
#3370=VERTEX_POINT('',#11313);
#3371=VERTEX_POINT('',#11317);
#3372=VERTEX_POINT('',#11319);
#3373=VERTEX_POINT('',#11323);
#3374=VERTEX_POINT('',#11325);
#3375=VERTEX_POINT('',#11329);
#3376=VERTEX_POINT('',#11331);
#3377=VERTEX_POINT('',#11335);
#3378=VERTEX_POINT('',#11337);
#3379=VERTEX_POINT('',#11341);
#3380=VERTEX_POINT('',#11343);
#3381=VERTEX_POINT('',#11347);
#3382=VERTEX_POINT('',#11349);
#3383=VERTEX_POINT('',#11353);
#3384=VERTEX_POINT('',#11355);
#3385=VERTEX_POINT('',#11359);
#3386=VERTEX_POINT('',#11361);
#3387=VERTEX_POINT('',#11365);
#3388=VERTEX_POINT('',#11367);
#3389=VERTEX_POINT('',#11371);
#3390=VERTEX_POINT('',#11373);
#3391=VERTEX_POINT('',#11377);
#3392=VERTEX_POINT('',#11379);
#3393=VERTEX_POINT('',#11383);
#3394=VERTEX_POINT('',#11385);
#3395=VERTEX_POINT('',#11389);
#3396=VERTEX_POINT('',#11391);
#3397=VERTEX_POINT('',#11401);
#3398=VERTEX_POINT('',#11403);
#3399=VERTEX_POINT('',#11407);
#3400=VERTEX_POINT('',#11408);
#3401=VERTEX_POINT('',#11412);
#3402=VERTEX_POINT('',#11427);
#3403=VERTEX_POINT('',#11429);
#3404=VERTEX_POINT('',#11432);
#3405=VERTEX_POINT('',#11452);
#3406=VERTEX_POINT('',#11453);
#3407=VERTEX_POINT('',#11455);
#3408=VERTEX_POINT('',#11457);
#3409=VERTEX_POINT('',#11459);
#3410=VERTEX_POINT('',#11462);
#3411=VERTEX_POINT('',#11465);
#3412=VERTEX_POINT('',#11467);
#3413=VERTEX_POINT('',#11471);
#3414=VERTEX_POINT('',#11473);
#3415=VERTEX_POINT('',#11481);
#3416=VERTEX_POINT('',#11485);
#3417=VERTEX_POINT('',#11491);
#3418=VERTEX_POINT('',#11493);
#3419=VERTEX_POINT('',#11498);
#3420=VERTEX_POINT('',#11500);
#3421=VERTEX_POINT('',#11507);
#3422=VERTEX_POINT('',#11508);
#3423=VERTEX_POINT('',#11510);
#3424=VERTEX_POINT('',#11512);
#3425=VERTEX_POINT('',#11516);
#3426=VERTEX_POINT('',#11518);
#3427=VERTEX_POINT('',#11522);
#3428=VERTEX_POINT('',#11524);
#3429=VERTEX_POINT('',#11528);
#3430=VERTEX_POINT('',#11530);
#3431=VERTEX_POINT('',#11534);
#3432=VERTEX_POINT('',#11536);
#3433=VERTEX_POINT('',#11544);
#3434=VERTEX_POINT('',#11547);
#3435=VERTEX_POINT('',#11551);
#3436=VERTEX_POINT('',#11555);
#3437=VERTEX_POINT('',#11561);
#3438=VERTEX_POINT('',#11564);
#3439=VERTEX_POINT('',#11568);
#3440=VERTEX_POINT('',#11572);
#3441=VERTEX_POINT('',#11576);
#3442=VERTEX_POINT('',#11579);
#3443=VERTEX_POINT('',#11583);
#3444=VERTEX_POINT('',#11587);
#3445=VERTEX_POINT('',#11592);
#3446=VERTEX_POINT('',#11593);
#3447=VERTEX_POINT('',#11595);
#3448=VERTEX_POINT('',#11597);
#3449=VERTEX_POINT('',#11601);
#3450=VERTEX_POINT('',#11603);
#3451=VERTEX_POINT('',#11607);
#3452=VERTEX_POINT('',#11609);
#3453=VERTEX_POINT('',#11613);
#3454=VERTEX_POINT('',#11615);
#3455=VERTEX_POINT('',#11619);
#3456=VERTEX_POINT('',#11621);
#3457=VERTEX_POINT('',#11687);
#3458=VERTEX_POINT('',#11689);
#3459=VERTEX_POINT('',#11693);
#3460=VERTEX_POINT('',#11694);
#3461=VERTEX_POINT('',#11696);
#3462=VERTEX_POINT('',#11698);
#3463=VERTEX_POINT('',#11702);
#3464=VERTEX_POINT('',#11704);
#3465=VERTEX_POINT('',#11708);
#3466=VERTEX_POINT('',#11712);
#3467=EDGE_CURVE('',#2942,#2942,#2719,.T.);
#3468=EDGE_CURVE('',#2942,#2943,#1697,.T.);
#3469=EDGE_CURVE('',#2943,#2943,#2720,.T.);
#3470=EDGE_CURVE('',#2944,#2944,#2721,.T.);
#3471=EDGE_CURVE('',#2944,#2945,#1698,.T.);
#3472=EDGE_CURVE('',#2945,#2945,#2722,.T.);
#3473=EDGE_CURVE('',#2946,#2946,#2723,.T.);
#3474=EDGE_CURVE('',#2946,#2947,#1699,.T.);
#3475=EDGE_CURVE('',#2947,#2947,#2724,.T.);
#3476=EDGE_CURVE('',#2948,#2948,#2725,.T.);
#3477=EDGE_CURVE('',#2948,#2949,#1700,.T.);
#3478=EDGE_CURVE('',#2949,#2949,#2726,.T.);
#3479=EDGE_CURVE('',#2950,#2950,#2727,.T.);
#3480=EDGE_CURVE('',#2950,#2951,#1701,.T.);
#3481=EDGE_CURVE('',#2951,#2951,#2728,.T.);
#3482=EDGE_CURVE('',#2952,#2952,#2729,.T.);
#3483=EDGE_CURVE('',#2952,#2953,#1702,.T.);
#3484=EDGE_CURVE('',#2953,#2953,#2730,.T.);
#3485=EDGE_CURVE('',#2954,#2954,#2731,.T.);
#3486=EDGE_CURVE('',#2954,#2955,#1703,.T.);
#3487=EDGE_CURVE('',#2955,#2955,#2732,.T.);
#3488=EDGE_CURVE('',#2956,#2956,#2733,.T.);
#3489=EDGE_CURVE('',#2956,#2957,#1704,.T.);
#3490=EDGE_CURVE('',#2957,#2957,#2734,.T.);
#3491=EDGE_CURVE('',#2958,#2958,#2735,.T.);
#3492=EDGE_CURVE('',#2958,#2959,#1705,.T.);
#3493=EDGE_CURVE('',#2959,#2959,#2736,.T.);
#3494=EDGE_CURVE('',#2960,#2960,#2737,.T.);
#3495=EDGE_CURVE('',#2960,#2961,#1706,.T.);
#3496=EDGE_CURVE('',#2961,#2961,#2738,.T.);
#3497=EDGE_CURVE('',#2962,#2963,#1707,.T.);
#3498=EDGE_CURVE('',#2963,#2964,#1708,.T.);
#3499=EDGE_CURVE('',#2965,#2964,#1709,.T.);
#3500=EDGE_CURVE('',#2962,#2965,#1710,.T.);
#3501=EDGE_CURVE('',#2966,#2962,#1711,.T.);
#3502=EDGE_CURVE('',#2967,#2965,#1712,.T.);
#3503=EDGE_CURVE('',#2966,#2967,#1713,.T.);
#3504=EDGE_CURVE('',#2968,#2966,#1714,.T.);
#3505=EDGE_CURVE('',#2969,#2967,#1715,.T.);
#3506=EDGE_CURVE('',#2968,#2969,#1716,.T.);
#3507=EDGE_CURVE('',#2963,#2968,#1717,.T.);
#3508=EDGE_CURVE('',#2964,#2969,#1718,.T.);
#3509=EDGE_CURVE('',#2970,#2971,#1719,.T.);
#3510=EDGE_CURVE('',#2971,#2972,#1720,.T.);
#3511=EDGE_CURVE('',#2973,#2972,#1721,.T.);
#3512=EDGE_CURVE('',#2970,#2973,#1722,.T.);
#3513=EDGE_CURVE('',#2974,#2970,#1723,.T.);
#3514=EDGE_CURVE('',#2975,#2973,#1724,.T.);
#3515=EDGE_CURVE('',#2974,#2975,#1725,.T.);
#3516=EDGE_CURVE('',#2976,#2974,#1726,.T.);
#3517=EDGE_CURVE('',#2977,#2975,#1727,.T.);
#3518=EDGE_CURVE('',#2976,#2977,#1728,.T.);
#3519=EDGE_CURVE('',#2971,#2976,#1729,.T.);
#3520=EDGE_CURVE('',#2972,#2977,#1730,.T.);
#3521=EDGE_CURVE('',#2978,#2979,#1731,.T.);
#3522=EDGE_CURVE('',#2979,#2980,#1732,.T.);
#3523=EDGE_CURVE('',#2981,#2980,#1733,.T.);
#3524=EDGE_CURVE('',#2978,#2981,#1734,.T.);
#3525=EDGE_CURVE('',#2982,#2978,#1735,.T.);
#3526=EDGE_CURVE('',#2983,#2981,#1736,.T.);
#3527=EDGE_CURVE('',#2982,#2983,#1737,.T.);
#3528=EDGE_CURVE('',#2984,#2982,#1738,.T.);
#3529=EDGE_CURVE('',#2985,#2983,#1739,.T.);
#3530=EDGE_CURVE('',#2984,#2985,#1740,.T.);
#3531=EDGE_CURVE('',#2979,#2984,#1741,.T.);
#3532=EDGE_CURVE('',#2980,#2985,#1742,.T.);
#3533=EDGE_CURVE('',#2986,#2986,#2739,.T.);
#3534=EDGE_CURVE('',#2986,#2987,#1743,.T.);
#3535=EDGE_CURVE('',#2987,#2987,#2740,.T.);
#3536=EDGE_CURVE('',#2988,#2988,#2741,.T.);
#3537=EDGE_CURVE('',#2989,#2989,#2742,.T.);
#3538=EDGE_CURVE('',#2989,#2990,#1744,.T.);
#3539=EDGE_CURVE('',#2990,#2990,#2743,.T.);
#3540=EDGE_CURVE('',#2991,#2991,#2744,.T.);
#3541=EDGE_CURVE('',#2992,#2992,#2745,.T.);
#3542=EDGE_CURVE('',#2992,#2988,#1745,.T.);
#3543=EDGE_CURVE('',#2993,#2993,#2746,.T.);
#3544=EDGE_CURVE('',#2993,#2991,#1746,.T.);
#3545=EDGE_CURVE('',#2994,#2994,#2747,.T.);
#3546=EDGE_CURVE('',#2994,#2995,#1747,.T.);
#3547=EDGE_CURVE('',#2995,#2995,#2748,.T.);
#3548=EDGE_CURVE('',#2996,#2996,#2749,.T.);
#3549=EDGE_CURVE('',#2997,#2997,#2750,.T.);
#3550=EDGE_CURVE('',#2997,#2998,#1748,.T.);
#3551=EDGE_CURVE('',#2998,#2998,#2751,.T.);
#3552=EDGE_CURVE('',#2999,#2999,#2752,.T.);
#3553=EDGE_CURVE('',#3000,#3000,#2753,.T.);
#3554=EDGE_CURVE('',#3000,#2996,#1749,.T.);
#3555=EDGE_CURVE('',#3001,#3001,#2754,.T.);
#3556=EDGE_CURVE('',#3001,#2999,#1750,.T.);
#3557=EDGE_CURVE('',#3002,#3002,#2755,.T.);
#3558=EDGE_CURVE('',#3002,#3003,#1751,.T.);
#3559=EDGE_CURVE('',#3003,#3003,#2756,.T.);
#3560=EDGE_CURVE('',#3004,#3004,#2757,.T.);
#3561=EDGE_CURVE('',#3004,#3005,#1752,.T.);
#3562=EDGE_CURVE('',#3005,#3005,#2758,.T.);
#3563=EDGE_CURVE('',#3006,#3007,#1753,.T.);
#3564=EDGE_CURVE('',#3007,#3008,#1754,.T.);
#3565=EDGE_CURVE('',#3009,#3008,#1755,.T.);
#3566=EDGE_CURVE('',#3006,#3009,#1756,.T.);
#3567=EDGE_CURVE('',#3010,#3006,#1757,.T.);
#3568=EDGE_CURVE('',#3011,#3009,#1758,.T.);
#3569=EDGE_CURVE('',#3010,#3011,#1759,.T.);
#3570=EDGE_CURVE('',#3012,#3010,#1760,.T.);
#3571=EDGE_CURVE('',#3013,#3011,#1761,.T.);
#3572=EDGE_CURVE('',#3012,#3013,#1762,.T.);
#3573=EDGE_CURVE('',#3007,#3012,#1763,.T.);
#3574=EDGE_CURVE('',#3008,#3013,#1764,.T.);
#3575=EDGE_CURVE('',#3014,#3014,#2759,.T.);
#3576=EDGE_CURVE('',#3014,#3015,#1765,.T.);
#3577=EDGE_CURVE('',#3015,#3015,#2760,.T.);
#3578=EDGE_CURVE('',#3016,#3016,#2761,.T.);
#3579=EDGE_CURVE('',#3016,#3017,#1766,.T.);
#3580=EDGE_CURVE('',#3017,#3017,#2762,.T.);
#3581=EDGE_CURVE('',#3018,#3018,#2763,.T.);
#3582=EDGE_CURVE('',#3018,#3019,#1767,.T.);
#3583=EDGE_CURVE('',#3019,#3019,#2764,.T.);
#3584=EDGE_CURVE('',#3020,#3020,#2765,.T.);
#3585=EDGE_CURVE('',#3020,#3021,#1768,.T.);
#3586=EDGE_CURVE('',#3021,#3021,#2766,.T.);
#3587=EDGE_CURVE('',#3022,#3022,#2767,.T.);
#3588=EDGE_CURVE('',#3022,#3023,#1769,.T.);
#3589=EDGE_CURVE('',#3023,#3023,#2768,.T.);
#3590=EDGE_CURVE('',#3024,#3024,#2769,.T.);
#3591=EDGE_CURVE('',#3025,#3025,#2770,.T.);
#3592=EDGE_CURVE('',#3025,#3026,#1770,.T.);
#3593=EDGE_CURVE('',#3026,#3026,#2771,.T.);
#3594=EDGE_CURVE('',#3027,#3027,#2772,.T.);
#3595=EDGE_CURVE('',#3028,#3028,#2773,.T.);
#3596=EDGE_CURVE('',#3028,#3024,#1771,.T.);
#3597=EDGE_CURVE('',#3029,#3029,#2774,.T.);
#3598=EDGE_CURVE('',#3029,#3027,#1772,.T.);
#3599=EDGE_CURVE('',#3030,#3030,#2775,.T.);
#3600=EDGE_CURVE('',#3030,#3031,#1773,.T.);
#3601=EDGE_CURVE('',#3031,#3031,#2776,.T.);
#3602=EDGE_CURVE('',#3032,#3032,#2777,.T.);
#3603=EDGE_CURVE('',#3033,#3033,#2778,.T.);
#3604=EDGE_CURVE('',#3033,#3034,#1774,.T.);
#3605=EDGE_CURVE('',#3034,#3034,#2779,.T.);
#3606=EDGE_CURVE('',#3035,#3035,#2780,.T.);
#3607=EDGE_CURVE('',#3036,#3036,#2781,.T.);
#3608=EDGE_CURVE('',#3036,#3032,#1775,.T.);
#3609=EDGE_CURVE('',#3037,#3037,#2782,.T.);
#3610=EDGE_CURVE('',#3037,#3035,#1776,.T.);
#3611=EDGE_CURVE('',#3038,#3038,#2783,.T.);
#3612=EDGE_CURVE('',#3038,#3039,#1777,.T.);
#3613=EDGE_CURVE('',#3039,#3039,#2784,.T.);
#3614=EDGE_CURVE('',#3040,#3040,#2785,.T.);
#3615=EDGE_CURVE('',#3040,#3041,#1778,.T.);
#3616=EDGE_CURVE('',#3041,#3041,#2786,.T.);
#3617=EDGE_CURVE('',#3042,#3043,#1779,.T.);
#3618=EDGE_CURVE('',#3043,#3044,#1780,.T.);
#3619=EDGE_CURVE('',#3045,#3044,#1781,.T.);
#3620=EDGE_CURVE('',#3042,#3045,#1782,.T.);
#3621=EDGE_CURVE('',#3046,#3042,#1783,.T.);
#3622=EDGE_CURVE('',#3047,#3045,#1784,.T.);
#3623=EDGE_CURVE('',#3046,#3047,#1785,.T.);
#3624=EDGE_CURVE('',#3048,#3046,#1786,.T.);
#3625=EDGE_CURVE('',#3049,#3047,#1787,.T.);
#3626=EDGE_CURVE('',#3048,#3049,#1788,.T.);
#3627=EDGE_CURVE('',#3043,#3048,#1789,.T.);
#3628=EDGE_CURVE('',#3044,#3049,#1790,.T.);
#3629=EDGE_CURVE('',#3050,#3050,#2787,.T.);
#3630=EDGE_CURVE('',#3050,#3051,#1791,.T.);
#3631=EDGE_CURVE('',#3051,#3051,#2788,.T.);
#3632=EDGE_CURVE('',#3052,#3052,#2789,.T.);
#3633=EDGE_CURVE('',#3052,#3053,#1792,.T.);
#3634=EDGE_CURVE('',#3053,#3053,#2790,.T.);
#3635=EDGE_CURVE('',#3054,#3054,#2791,.T.);
#3636=EDGE_CURVE('',#3054,#3055,#1793,.T.);
#3637=EDGE_CURVE('',#3055,#3055,#2792,.T.);
#3638=EDGE_CURVE('',#3056,#3056,#2793,.T.);
#3639=EDGE_CURVE('',#3056,#3057,#1794,.T.);
#3640=EDGE_CURVE('',#3057,#3057,#2794,.T.);
#3641=EDGE_CURVE('',#3058,#3058,#2795,.T.);
#3642=EDGE_CURVE('',#3058,#3059,#1795,.T.);
#3643=EDGE_CURVE('',#3059,#3059,#2796,.T.);
#3644=EDGE_CURVE('',#3060,#3060,#2797,.T.);
#3645=EDGE_CURVE('',#3060,#3061,#1796,.T.);
#3646=EDGE_CURVE('',#3061,#3061,#2798,.T.);
#3647=EDGE_CURVE('',#3062,#3062,#2799,.T.);
#3648=EDGE_CURVE('',#3062,#3063,#1797,.T.);
#3649=EDGE_CURVE('',#3063,#3063,#2800,.T.);
#3650=EDGE_CURVE('',#3064,#3065,#1798,.T.);
#3651=EDGE_CURVE('',#3064,#3066,#1799,.T.);
#3652=EDGE_CURVE('',#3067,#3066,#1800,.T.);
#3653=EDGE_CURVE('',#3065,#3067,#1801,.T.);
#3654=EDGE_CURVE('',#3068,#3069,#1802,.T.);
#3655=EDGE_CURVE('',#3070,#3068,#1803,.T.);
#3656=EDGE_CURVE('',#3071,#3070,#1804,.T.);
#3657=EDGE_CURVE('',#3069,#3071,#1805,.T.);
#3658=EDGE_CURVE('',#3065,#3072,#1806,.T.);
#3659=EDGE_CURVE('',#3073,#3067,#1807,.T.);
#3660=EDGE_CURVE('',#3072,#3073,#1808,.T.);
#3661=EDGE_CURVE('',#3074,#3064,#1809,.T.);
#3662=EDGE_CURVE('',#3074,#3075,#1810,.T.);
#3663=EDGE_CURVE('',#3066,#3075,#1811,.T.);
#3664=EDGE_CURVE('',#3075,#3073,#1812,.T.);
#3665=EDGE_CURVE('',#3072,#3074,#1813,.T.);
#3666=EDGE_CURVE('',#3070,#3076,#1814,.T.);
#3667=EDGE_CURVE('',#3077,#3076,#1815,.T.);
#3668=EDGE_CURVE('',#3071,#3077,#1816,.T.);
#3669=EDGE_CURVE('',#3068,#3078,#1817,.T.);
#3670=EDGE_CURVE('',#3076,#3078,#1818,.T.);
#3671=EDGE_CURVE('',#3069,#3079,#1819,.T.);
#3672=EDGE_CURVE('',#3078,#3079,#1820,.T.);
#3673=EDGE_CURVE('',#3079,#3077,#1821,.T.);
#3674=EDGE_CURVE('',#3080,#3080,#2801,.T.);
#3675=EDGE_CURVE('',#3080,#3081,#1822,.T.);
#3676=EDGE_CURVE('',#3081,#3081,#2802,.T.);
#3677=EDGE_CURVE('',#3082,#3082,#2803,.T.);
#3678=EDGE_CURVE('',#3083,#3083,#2804,.T.);
#3679=EDGE_CURVE('',#3082,#3084,#1823,.T.);
#3680=EDGE_CURVE('',#3084,#3084,#2805,.T.);
#3681=EDGE_CURVE('',#3085,#3085,#2806,.T.);
#3682=EDGE_CURVE('',#3085,#3083,#1824,.T.);
#3683=EDGE_CURVE('',#3086,#3086,#2807,.T.);
#3684=EDGE_CURVE('',#3086,#3087,#1825,.T.);
#3685=EDGE_CURVE('',#3087,#3087,#2808,.T.);
#3686=EDGE_CURVE('',#3088,#3088,#2809,.T.);
#3687=EDGE_CURVE('',#3088,#3089,#1826,.T.);
#3688=EDGE_CURVE('',#3089,#3089,#2810,.T.);
#3689=EDGE_CURVE('',#3090,#3090,#2811,.T.);
#3690=EDGE_CURVE('',#3090,#3091,#1827,.T.);
#3691=EDGE_CURVE('',#3091,#3091,#2812,.T.);
#3692=EDGE_CURVE('',#3092,#3092,#2813,.T.);
#3693=EDGE_CURVE('',#3092,#3093,#1828,.T.);
#3694=EDGE_CURVE('',#3093,#3093,#2814,.T.);
#3695=EDGE_CURVE('',#3094,#3095,#1829,.T.);
#3696=EDGE_CURVE('',#3094,#3096,#1830,.T.);
#3697=EDGE_CURVE('',#3097,#3096,#1831,.T.);
#3698=EDGE_CURVE('',#3095,#3097,#1832,.T.);
#3699=EDGE_CURVE('',#3095,#3098,#1833,.T.);
#3700=EDGE_CURVE('',#3099,#3097,#1834,.T.);
#3701=EDGE_CURVE('',#3098,#3099,#1835,.T.);
#3702=EDGE_CURVE('',#3098,#3100,#1836,.T.);
#3703=EDGE_CURVE('',#3101,#3099,#1837,.T.);
#3704=EDGE_CURVE('',#3100,#3101,#1838,.T.);
#3705=EDGE_CURVE('',#3100,#3094,#1839,.T.);
#3706=EDGE_CURVE('',#3096,#3101,#1840,.T.);
#3707=EDGE_CURVE('',#3102,#3102,#2815,.T.);
#3708=EDGE_CURVE('',#3102,#3103,#1841,.T.);
#3709=EDGE_CURVE('',#3103,#3103,#2816,.T.);
#3710=EDGE_CURVE('',#3104,#3105,#1842,.T.);
#3711=EDGE_CURVE('',#3105,#3106,#1843,.T.);
#3712=EDGE_CURVE('',#3107,#3106,#1844,.T.);
#3713=EDGE_CURVE('',#3104,#3107,#1845,.T.);
#3714=EDGE_CURVE('',#3108,#3104,#1846,.T.);
#3715=EDGE_CURVE('',#3109,#3107,#1847,.T.);
#3716=EDGE_CURVE('',#3108,#3109,#1848,.T.);
#3717=EDGE_CURVE('',#3110,#3108,#1849,.T.);
#3718=EDGE_CURVE('',#3111,#3109,#1850,.T.);
#3719=EDGE_CURVE('',#3110,#3111,#1851,.T.);
#3720=EDGE_CURVE('',#3105,#3110,#1852,.T.);
#3721=EDGE_CURVE('',#3106,#3111,#1853,.T.);
#3722=EDGE_CURVE('',#3112,#3112,#2817,.T.);
#3723=EDGE_CURVE('',#3112,#3113,#1854,.T.);
#3724=EDGE_CURVE('',#3113,#3113,#2818,.T.);
#3725=EDGE_CURVE('',#3114,#3114,#2819,.T.);
#3726=EDGE_CURVE('',#3114,#3115,#1855,.T.);
#3727=EDGE_CURVE('',#3115,#3115,#2820,.T.);
#3728=EDGE_CURVE('',#3116,#3117,#2821,.T.);
#3729=EDGE_CURVE('',#3118,#3119,#1856,.T.);
#3730=EDGE_CURVE('',#3118,#3120,#1857,.T.);
#3731=EDGE_CURVE('',#3119,#3120,#2822,.T.);
#3732=EDGE_CURVE('',#3121,#3122,#1858,.T.);
#3733=EDGE_CURVE('',#3123,#3121,#2823,.T.);
#3734=EDGE_CURVE('',#3123,#3122,#1859,.T.);
#3735=EDGE_CURVE('',#3124,#3125,#1860,.T.);
#3736=EDGE_CURVE('',#3126,#3124,#2824,.T.);
#3737=EDGE_CURVE('',#3126,#3125,#1861,.T.);
#3738=EDGE_CURVE('',#3125,#3118,#1862,.T.);
#3739=EDGE_CURVE('',#3120,#3126,#1863,.T.);
#3740=EDGE_CURVE('',#3127,#3128,#1864,.T.);
#3741=EDGE_CURVE('',#3127,#3129,#1865,.T.);
#3742=EDGE_CURVE('',#3128,#3129,#2825,.T.);
#3743=EDGE_CURVE('',#3122,#3127,#1866,.T.);
#3744=EDGE_CURVE('',#3129,#3123,#1867,.T.);
#3745=EDGE_CURVE('',#3130,#3131,#1868,.T.);
#3746=EDGE_CURVE('',#3131,#3132,#1869,.T.);
#3747=EDGE_CURVE('',#3132,#3133,#1870,.T.);
#3748=EDGE_CURVE('',#3133,#3130,#1871,.T.);
#3749=EDGE_CURVE('',#3134,#3134,#2826,.T.);
#3750=EDGE_CURVE('',#3135,#3135,#2827,.T.);
#3751=EDGE_CURVE('',#3128,#3136,#1872,.T.);
#3752=EDGE_CURVE('',#3136,#3137,#1873,.T.);
#3753=EDGE_CURVE('',#3137,#3124,#1874,.T.);
#3754=EDGE_CURVE('',#3119,#3138,#1875,.T.);
#3755=EDGE_CURVE('',#3138,#3139,#1876,.T.);
#3756=EDGE_CURVE('',#3139,#3121,#1877,.T.);
#3757=EDGE_CURVE('',#3138,#3139,#2828,.T.);
#3758=EDGE_CURVE('',#3136,#3137,#2829,.T.);
#3759=EDGE_CURVE('',#3140,#3141,#1878,.T.);
#3760=EDGE_CURVE('',#3140,#3142,#1879,.T.);
#3761=EDGE_CURVE('',#3142,#3143,#1880,.T.);
#3762=EDGE_CURVE('',#3141,#3143,#1881,.T.);
#3763=EDGE_CURVE('',#3144,#3140,#1882,.T.);
#3764=EDGE_CURVE('',#3144,#3145,#1883,.T.);
#3765=EDGE_CURVE('',#3145,#3142,#1884,.T.);
#3766=EDGE_CURVE('',#3146,#3144,#1885,.T.);
#3767=EDGE_CURVE('',#3146,#3147,#1886,.T.);
#3768=EDGE_CURVE('',#3147,#3145,#1887,.T.);
#3769=EDGE_CURVE('',#3141,#3146,#1888,.T.);
#3770=EDGE_CURVE('',#3143,#3147,#1889,.T.);
#3771=EDGE_CURVE('',#3148,#3148,#2830,.T.);
#3772=EDGE_CURVE('',#3148,#3135,#1890,.T.);
#3773=EDGE_CURVE('',#3149,#3149,#2831,.T.);
#3774=EDGE_CURVE('',#3149,#3134,#1891,.T.);
#3775=EDGE_CURVE('',#3150,#3151,#1892,.T.);
#3776=EDGE_CURVE('',#3151,#3130,#1893,.T.);
#3777=EDGE_CURVE('',#3150,#3133,#1894,.T.);
#3778=EDGE_CURVE('',#3152,#3150,#1895,.T.);
#3779=EDGE_CURVE('',#3152,#3132,#1896,.T.);
#3780=EDGE_CURVE('',#3153,#3152,#1897,.T.);
#3781=EDGE_CURVE('',#3153,#3131,#1898,.T.);
#3782=EDGE_CURVE('',#3151,#3153,#1899,.T.);
#3783=EDGE_CURVE('',#3154,#3154,#2832,.T.);
#3784=EDGE_CURVE('',#3154,#3155,#1900,.T.);
#3785=EDGE_CURVE('',#3155,#3155,#2833,.T.);
#3786=EDGE_CURVE('',#3156,#3156,#2834,.T.);
#3787=EDGE_CURVE('',#3157,#3158,#2835,.T.);
#3788=EDGE_CURVE('',#3159,#3159,#2836,.T.);
#3789=EDGE_CURVE('',#3160,#3161,#273,.T.);
#3790=EDGE_CURVE('',#3162,#3160,#274,.T.);
#3791=EDGE_CURVE('',#3161,#3162,#275,.T.);
#3792=EDGE_CURVE('',#3161,#3163,#1901,.T.);
#3793=EDGE_CURVE('',#3163,#3163,#276,.T.);
#3794=EDGE_CURVE('',#3164,#3164,#277,.T.);
#3795=EDGE_CURVE('',#3164,#3165,#1902,.T.);
#3796=EDGE_CURVE('',#3166,#3165,#278,.T.);
#3797=EDGE_CURVE('',#3167,#3166,#279,.T.);
#3798=EDGE_CURVE('',#3165,#3167,#280,.T.);
#3799=EDGE_CURVE('',#3168,#3168,#2837,.T.);
#3800=EDGE_CURVE('',#3168,#3169,#1903,.T.);
#3801=EDGE_CURVE('',#3169,#3169,#2838,.T.);
#3802=EDGE_CURVE('',#3170,#3171,#281,.T.);
#3803=EDGE_CURVE('',#3171,#3172,#282,.T.);
#3804=EDGE_CURVE('',#3172,#3170,#283,.T.);
#3805=EDGE_CURVE('',#3173,#3174,#284,.T.);
#3806=EDGE_CURVE('',#3174,#3175,#285,.T.);
#3807=EDGE_CURVE('',#3175,#3173,#286,.T.);
#3808=EDGE_CURVE('',#3176,#3177,#287,.T.);
#3809=EDGE_CURVE('',#3177,#3178,#288,.T.);
#3810=EDGE_CURVE('',#3178,#3176,#289,.T.);
#3811=EDGE_CURVE('',#3179,#3180,#290,.T.);
#3812=EDGE_CURVE('',#3180,#3181,#291,.T.);
#3813=EDGE_CURVE('',#3181,#3179,#292,.T.);
#3814=EDGE_CURVE('',#3172,#3182,#1904,.T.);
#3815=EDGE_CURVE('',#3182,#3182,#293,.T.);
#3816=EDGE_CURVE('',#3183,#3183,#294,.T.);
#3817=EDGE_CURVE('',#3183,#3175,#1905,.T.);
#3818=EDGE_CURVE('',#3178,#3184,#1906,.T.);
#3819=EDGE_CURVE('',#3184,#3184,#295,.T.);
#3820=EDGE_CURVE('',#3185,#3185,#296,.T.);
#3821=EDGE_CURVE('',#3185,#3181,#1907,.T.);
#3822=EDGE_CURVE('',#3186,#3186,#2839,.T.);
#3823=EDGE_CURVE('',#3187,#3187,#2840,.T.);
#3824=EDGE_CURVE('',#3188,#3188,#2841,.T.);
#3825=EDGE_CURVE('',#3188,#3187,#1908,.T.);
#3826=EDGE_CURVE('',#3189,#3189,#2842,.T.);
#3827=EDGE_CURVE('',#3189,#3186,#1909,.T.);
#3828=EDGE_CURVE('',#3190,#3190,#2843,.T.);
#3829=EDGE_CURVE('',#3190,#3191,#1910,.T.);
#3830=EDGE_CURVE('',#3191,#3191,#2844,.T.);
#3831=EDGE_CURVE('',#3192,#3192,#2845,.T.);
#3832=EDGE_CURVE('',#3192,#3193,#1911,.T.);
#3833=EDGE_CURVE('',#3193,#3193,#2846,.T.);
#3834=EDGE_CURVE('',#3194,#3195,#1912,.T.);
#3835=EDGE_CURVE('',#3195,#3196,#1913,.T.);
#3836=EDGE_CURVE('',#3196,#3197,#1914,.T.);
#3837=EDGE_CURVE('',#3194,#3197,#1915,.T.);
#3838=EDGE_CURVE('',#3195,#3198,#1916,.T.);
#3839=EDGE_CURVE('',#3198,#3199,#1917,.T.);
#3840=EDGE_CURVE('',#3199,#3196,#1918,.T.);
#3841=EDGE_CURVE('',#3198,#3200,#1919,.T.);
#3842=EDGE_CURVE('',#3200,#3201,#1920,.T.);
#3843=EDGE_CURVE('',#3201,#3199,#1921,.T.);
#3844=EDGE_CURVE('',#3200,#3202,#1922,.T.);
#3845=EDGE_CURVE('',#3202,#3203,#1923,.T.);
#3846=EDGE_CURVE('',#3203,#3201,#1924,.T.);
#3847=EDGE_CURVE('',#3202,#3204,#1925,.T.);
#3848=EDGE_CURVE('',#3204,#3205,#1926,.T.);
#3849=EDGE_CURVE('',#3205,#3203,#1927,.T.);
#3850=EDGE_CURVE('',#3204,#3194,#1928,.T.);
#3851=EDGE_CURVE('',#3197,#3205,#1929,.T.);
#3852=EDGE_CURVE('',#3206,#3206,#2847,.T.);
#3853=EDGE_CURVE('',#3207,#3207,#2848,.T.);
#3854=EDGE_CURVE('',#3208,#3208,#2849,.T.);
#3855=EDGE_CURVE('',#3208,#3207,#1930,.T.);
#3856=EDGE_CURVE('',#3209,#3209,#2850,.T.);
#3857=EDGE_CURVE('',#3209,#3208,#1931,.T.);
#3858=EDGE_CURVE('',#3210,#3210,#2851,.T.);
#3859=EDGE_CURVE('',#3210,#3209,#1932,.T.);
#3860=EDGE_CURVE('',#3211,#3211,#2852,.T.);
#3861=EDGE_CURVE('',#3212,#3212,#2853,.F.);
#3862=EDGE_CURVE('',#3212,#3211,#1933,.T.);
#3863=EDGE_CURVE('',#3206,#3212,#1934,.T.);
#3864=EDGE_CURVE('',#3213,#3214,#1935,.T.);
#3865=EDGE_CURVE('',#3214,#3215,#1936,.T.);
#3866=EDGE_CURVE('',#3215,#3216,#1937,.T.);
#3867=EDGE_CURVE('',#3213,#3216,#1938,.T.);
#3868=EDGE_CURVE('',#3214,#3217,#1939,.T.);
#3869=EDGE_CURVE('',#3217,#3218,#1940,.T.);
#3870=EDGE_CURVE('',#3218,#3215,#1941,.T.);
#3871=EDGE_CURVE('',#3217,#3219,#1942,.T.);
#3872=EDGE_CURVE('',#3219,#3220,#1943,.T.);
#3873=EDGE_CURVE('',#3220,#3218,#1944,.T.);
#3874=EDGE_CURVE('',#3219,#3221,#1945,.T.);
#3875=EDGE_CURVE('',#3221,#3222,#1946,.T.);
#3876=EDGE_CURVE('',#3222,#3220,#1947,.T.);
#3877=EDGE_CURVE('',#3221,#3223,#1948,.T.);
#3878=EDGE_CURVE('',#3223,#3224,#1949,.T.);
#3879=EDGE_CURVE('',#3224,#3222,#1950,.T.);
#3880=EDGE_CURVE('',#3223,#3213,#1951,.T.);
#3881=EDGE_CURVE('',#3216,#3224,#1952,.T.);
#3882=EDGE_CURVE('',#3225,#3225,#2854,.T.);
#3883=EDGE_CURVE('',#3226,#3226,#2855,.T.);
#3884=EDGE_CURVE('',#3227,#3227,#2856,.T.);
#3885=EDGE_CURVE('',#3227,#3226,#1953,.T.);
#3886=EDGE_CURVE('',#3228,#3228,#2857,.T.);
#3887=EDGE_CURVE('',#3228,#3227,#1954,.T.);
#3888=EDGE_CURVE('',#3229,#3229,#2858,.T.);
#3889=EDGE_CURVE('',#3229,#3228,#1955,.T.);
#3890=EDGE_CURVE('',#3230,#3230,#2859,.T.);
#3891=EDGE_CURVE('',#3231,#3231,#2860,.F.);
#3892=EDGE_CURVE('',#3231,#3230,#1956,.T.);
#3893=EDGE_CURVE('',#3225,#3231,#1957,.T.);
#3894=EDGE_CURVE('',#3232,#3232,#2861,.T.);
#3895=EDGE_CURVE('',#3232,#3233,#1958,.T.);
#3896=EDGE_CURVE('',#3233,#3233,#2862,.T.);
#3897=EDGE_CURVE('',#3234,#3235,#1959,.T.);
#3898=EDGE_CURVE('',#3234,#3235,#2863,.T.);
#3899=EDGE_CURVE('',#3236,#3234,#297,.T.);
#3900=EDGE_CURVE('',#3237,#3236,#2864,.T.);
#3901=EDGE_CURVE('',#3237,#3238,#1960,.T.);
#3902=EDGE_CURVE('',#3239,#3238,#298,.T.);
#3903=EDGE_CURVE('',#3238,#3239,#299,.T.);
#3904=EDGE_CURVE('',#3240,#3237,#2865,.T.);
#3905=EDGE_CURVE('',#3235,#3240,#300,.T.);
#3906=EDGE_CURVE('',#3240,#3236,#1961,.T.);
#3907=EDGE_CURVE('',#3241,#3241,#2866,.T.);
#3908=EDGE_CURVE('',#3241,#3242,#1962,.T.);
#3909=EDGE_CURVE('',#3242,#3242,#2867,.T.);
#3910=EDGE_CURVE('',#3243,#3243,#2868,.T.);
#3911=EDGE_CURVE('',#3243,#3244,#1963,.T.);
#3912=EDGE_CURVE('',#3244,#3244,#2869,.T.);
#3913=EDGE_CURVE('',#3245,#3246,#1964,.T.);
#3914=EDGE_CURVE('',#3245,#3246,#2870,.T.);
#3915=EDGE_CURVE('',#3247,#3245,#301,.T.);
#3916=EDGE_CURVE('',#3248,#3247,#2871,.T.);
#3917=EDGE_CURVE('',#3248,#3249,#1965,.T.);
#3918=EDGE_CURVE('',#3250,#3249,#302,.T.);
#3919=EDGE_CURVE('',#3249,#3250,#303,.T.);
#3920=EDGE_CURVE('',#3251,#3248,#2872,.T.);
#3921=EDGE_CURVE('',#3246,#3251,#304,.T.);
#3922=EDGE_CURVE('',#3251,#3247,#1966,.T.);
#3923=EDGE_CURVE('',#3252,#3252,#2873,.T.);
#3924=EDGE_CURVE('',#3252,#3253,#1967,.T.);
#3925=EDGE_CURVE('',#3253,#3253,#2874,.T.);
#3926=EDGE_CURVE('',#3254,#3254,#2875,.T.);
#3927=EDGE_CURVE('',#3254,#3255,#1968,.T.);
#3928=EDGE_CURVE('',#3255,#3255,#2876,.T.);
#3929=EDGE_CURVE('',#3256,#3256,#2877,.T.);
#3930=EDGE_CURVE('',#3256,#3257,#1969,.T.);
#3931=EDGE_CURVE('',#3257,#3257,#2878,.T.);
#3932=EDGE_CURVE('',#3258,#3258,#2879,.T.);
#3933=EDGE_CURVE('',#3258,#3259,#1970,.T.);
#3934=EDGE_CURVE('',#3259,#3259,#2880,.T.);
#3935=EDGE_CURVE('',#3260,#3260,#2881,.T.);
#3936=EDGE_CURVE('',#3260,#3261,#1971,.T.);
#3937=EDGE_CURVE('',#3261,#3261,#2882,.T.);
#3938=EDGE_CURVE('',#3262,#3262,#2883,.T.);
#3939=EDGE_CURVE('',#3262,#3263,#1972,.T.);
#3940=EDGE_CURVE('',#3263,#3263,#2884,.T.);
#3941=EDGE_CURVE('',#3264,#3265,#1973,.T.);
#3942=EDGE_CURVE('',#3264,#3265,#2885,.T.);
#3943=EDGE_CURVE('',#3266,#3264,#305,.T.);
#3944=EDGE_CURVE('',#3267,#3266,#2886,.T.);
#3945=EDGE_CURVE('',#3267,#3268,#1974,.T.);
#3946=EDGE_CURVE('',#3269,#3268,#306,.T.);
#3947=EDGE_CURVE('',#3268,#3269,#307,.T.);
#3948=EDGE_CURVE('',#3270,#3267,#2887,.T.);
#3949=EDGE_CURVE('',#3265,#3270,#308,.T.);
#3950=EDGE_CURVE('',#3270,#3266,#1975,.T.);
#3951=EDGE_CURVE('',#3271,#3271,#2888,.T.);
#3952=EDGE_CURVE('',#3271,#3272,#1976,.T.);
#3953=EDGE_CURVE('',#3272,#3272,#2889,.T.);
#3954=EDGE_CURVE('',#3273,#3273,#2890,.T.);
#3955=EDGE_CURVE('',#3273,#3274,#1977,.T.);
#3956=EDGE_CURVE('',#3274,#3274,#2891,.T.);
#3957=EDGE_CURVE('',#3275,#3275,#2892,.T.);
#3958=EDGE_CURVE('',#3275,#3276,#1978,.T.);
#3959=EDGE_CURVE('',#3276,#3276,#2893,.T.);
#3960=EDGE_CURVE('',#3277,#3277,#2894,.T.);
#3961=EDGE_CURVE('',#3277,#3278,#1979,.T.);
#3962=EDGE_CURVE('',#3278,#3278,#2895,.T.);
#3963=EDGE_CURVE('',#3279,#3280,#1980,.T.);
#3964=EDGE_CURVE('',#3279,#3280,#2896,.T.);
#3965=EDGE_CURVE('',#3281,#3279,#309,.T.);
#3966=EDGE_CURVE('',#3282,#3281,#2897,.T.);
#3967=EDGE_CURVE('',#3282,#3283,#1981,.T.);
#3968=EDGE_CURVE('',#3284,#3283,#310,.T.);
#3969=EDGE_CURVE('',#3283,#3284,#311,.T.);
#3970=EDGE_CURVE('',#3285,#3282,#2898,.T.);
#3971=EDGE_CURVE('',#3280,#3285,#312,.T.);
#3972=EDGE_CURVE('',#3285,#3281,#1982,.T.);
#3973=EDGE_CURVE('',#3286,#3286,#2899,.T.);
#3974=EDGE_CURVE('',#3286,#3287,#1983,.T.);
#3975=EDGE_CURVE('',#3287,#3287,#2900,.T.);
#3976=EDGE_CURVE('',#3288,#3288,#2901,.T.);
#3977=EDGE_CURVE('',#3288,#3289,#1984,.T.);
#3978=EDGE_CURVE('',#3289,#3289,#2902,.T.);
#3979=EDGE_CURVE('',#3290,#3291,#1985,.T.);
#3980=EDGE_CURVE('',#3290,#3291,#2903,.T.);
#3981=EDGE_CURVE('',#3292,#3290,#313,.T.);
#3982=EDGE_CURVE('',#3293,#3292,#2904,.T.);
#3983=EDGE_CURVE('',#3293,#3294,#1986,.T.);
#3984=EDGE_CURVE('',#3295,#3294,#314,.T.);
#3985=EDGE_CURVE('',#3294,#3295,#315,.T.);
#3986=EDGE_CURVE('',#3296,#3293,#2905,.T.);
#3987=EDGE_CURVE('',#3291,#3296,#316,.T.);
#3988=EDGE_CURVE('',#3296,#3292,#1987,.T.);
#3989=EDGE_CURVE('',#3297,#3297,#2906,.T.);
#3990=EDGE_CURVE('',#3297,#3298,#1988,.T.);
#3991=EDGE_CURVE('',#3298,#3298,#2907,.T.);
#3992=EDGE_CURVE('',#3299,#3299,#2908,.T.);
#3993=EDGE_CURVE('',#3300,#3300,#2909,.T.);
#3994=EDGE_CURVE('',#3300,#3299,#1989,.T.);
#3995=EDGE_CURVE('',#3301,#3302,#1990,.T.);
#3996=EDGE_CURVE('',#3301,#3303,#1991,.T.);
#3997=EDGE_CURVE('',#3304,#3303,#1992,.T.);
#3998=EDGE_CURVE('',#3302,#3304,#1993,.T.);
#3999=EDGE_CURVE('',#3302,#3305,#1994,.T.);
#4000=EDGE_CURVE('',#3306,#3304,#1995,.T.);
#4001=EDGE_CURVE('',#3305,#3306,#1996,.T.);
#4002=EDGE_CURVE('',#3305,#3307,#1997,.T.);
#4003=EDGE_CURVE('',#3308,#3306,#1998,.T.);
#4004=EDGE_CURVE('',#3307,#3308,#1999,.T.);
#4005=EDGE_CURVE('',#3307,#3309,#2000,.T.);
#4006=EDGE_CURVE('',#3310,#3308,#2001,.T.);
#4007=EDGE_CURVE('',#3309,#3310,#2002,.T.);
#4008=EDGE_CURVE('',#3309,#3311,#2003,.T.);
#4009=EDGE_CURVE('',#3312,#3310,#2004,.T.);
#4010=EDGE_CURVE('',#3311,#3312,#2005,.T.);
#4011=EDGE_CURVE('',#3311,#3313,#2006,.T.);
#4012=EDGE_CURVE('',#3314,#3312,#2007,.T.);
#4013=EDGE_CURVE('',#3313,#3314,#2008,.T.);
#4014=EDGE_CURVE('',#3313,#3315,#2009,.T.);
#4015=EDGE_CURVE('',#3316,#3314,#2010,.T.);
#4016=EDGE_CURVE('',#3315,#3316,#2011,.T.);
#4017=EDGE_CURVE('',#3315,#3317,#2012,.T.);
#4018=EDGE_CURVE('',#3318,#3316,#2013,.T.);
#4019=EDGE_CURVE('',#3317,#3318,#2014,.T.);
#4020=EDGE_CURVE('',#3317,#3319,#2015,.T.);
#4021=EDGE_CURVE('',#3320,#3318,#2016,.T.);
#4022=EDGE_CURVE('',#3319,#3320,#2017,.T.);
#4023=EDGE_CURVE('',#3319,#3321,#2018,.T.);
#4024=EDGE_CURVE('',#3322,#3320,#2019,.T.);
#4025=EDGE_CURVE('',#3321,#3322,#2020,.T.);
#4026=EDGE_CURVE('',#3321,#3323,#2021,.T.);
#4027=EDGE_CURVE('',#3324,#3322,#2022,.T.);
#4028=EDGE_CURVE('',#3323,#3324,#2023,.T.);
#4029=EDGE_CURVE('',#3323,#3325,#2024,.T.);
#4030=EDGE_CURVE('',#3326,#3324,#2025,.T.);
#4031=EDGE_CURVE('',#3325,#3326,#2026,.T.);
#4032=EDGE_CURVE('',#3325,#3327,#2027,.T.);
#4033=EDGE_CURVE('',#3328,#3326,#2028,.T.);
#4034=EDGE_CURVE('',#3327,#3328,#2029,.T.);
#4035=EDGE_CURVE('',#3327,#3329,#2030,.T.);
#4036=EDGE_CURVE('',#3330,#3328,#2031,.T.);
#4037=EDGE_CURVE('',#3329,#3330,#2032,.T.);
#4038=EDGE_CURVE('',#3329,#3331,#2033,.T.);
#4039=EDGE_CURVE('',#3332,#3330,#2034,.T.);
#4040=EDGE_CURVE('',#3331,#3332,#2035,.T.);
#4041=EDGE_CURVE('',#3331,#3333,#2036,.T.);
#4042=EDGE_CURVE('',#3334,#3332,#2037,.T.);
#4043=EDGE_CURVE('',#3333,#3334,#2038,.T.);
#4044=EDGE_CURVE('',#3333,#3335,#2039,.T.);
#4045=EDGE_CURVE('',#3336,#3334,#2040,.T.);
#4046=EDGE_CURVE('',#3335,#3336,#2041,.T.);
#4047=EDGE_CURVE('',#3335,#3337,#2042,.T.);
#4048=EDGE_CURVE('',#3338,#3336,#2043,.T.);
#4049=EDGE_CURVE('',#3337,#3338,#2044,.T.);
#4050=EDGE_CURVE('',#3337,#3339,#2045,.T.);
#4051=EDGE_CURVE('',#3340,#3338,#2046,.T.);
#4052=EDGE_CURVE('',#3339,#3340,#2047,.T.);
#4053=EDGE_CURVE('',#3339,#3341,#2048,.T.);
#4054=EDGE_CURVE('',#3342,#3340,#2049,.T.);
#4055=EDGE_CURVE('',#3341,#3342,#2050,.T.);
#4056=EDGE_CURVE('',#3341,#3343,#2051,.T.);
#4057=EDGE_CURVE('',#3344,#3342,#2052,.T.);
#4058=EDGE_CURVE('',#3343,#3344,#2053,.T.);
#4059=EDGE_CURVE('',#3343,#3345,#2054,.T.);
#4060=EDGE_CURVE('',#3346,#3344,#2055,.T.);
#4061=EDGE_CURVE('',#3345,#3346,#2056,.T.);
#4062=EDGE_CURVE('',#3345,#3347,#2057,.T.);
#4063=EDGE_CURVE('',#3348,#3346,#2058,.T.);
#4064=EDGE_CURVE('',#3347,#3348,#2059,.T.);
#4065=EDGE_CURVE('',#3347,#3349,#2060,.T.);
#4066=EDGE_CURVE('',#3350,#3348,#2061,.T.);
#4067=EDGE_CURVE('',#3349,#3350,#2062,.T.);
#4068=EDGE_CURVE('',#3349,#3351,#2063,.T.);
#4069=EDGE_CURVE('',#3352,#3350,#2064,.T.);
#4070=EDGE_CURVE('',#3351,#3352,#2065,.T.);
#4071=EDGE_CURVE('',#3351,#3353,#2066,.T.);
#4072=EDGE_CURVE('',#3354,#3352,#2067,.T.);
#4073=EDGE_CURVE('',#3353,#3354,#2068,.T.);
#4074=EDGE_CURVE('',#3353,#3355,#2069,.T.);
#4075=EDGE_CURVE('',#3356,#3354,#2070,.T.);
#4076=EDGE_CURVE('',#3355,#3356,#2071,.T.);
#4077=EDGE_CURVE('',#3355,#3357,#2072,.T.);
#4078=EDGE_CURVE('',#3358,#3356,#2073,.T.);
#4079=EDGE_CURVE('',#3357,#3358,#2074,.T.);
#4080=EDGE_CURVE('',#3357,#3359,#2075,.T.);
#4081=EDGE_CURVE('',#3360,#3358,#2076,.T.);
#4082=EDGE_CURVE('',#3359,#3360,#2077,.T.);
#4083=EDGE_CURVE('',#3359,#3361,#2078,.T.);
#4084=EDGE_CURVE('',#3362,#3360,#2079,.T.);
#4085=EDGE_CURVE('',#3361,#3362,#2080,.T.);
#4086=EDGE_CURVE('',#3361,#3363,#2081,.T.);
#4087=EDGE_CURVE('',#3364,#3362,#2082,.T.);
#4088=EDGE_CURVE('',#3363,#3364,#2083,.T.);
#4089=EDGE_CURVE('',#3363,#3365,#2084,.T.);
#4090=EDGE_CURVE('',#3366,#3364,#2085,.T.);
#4091=EDGE_CURVE('',#3365,#3366,#2086,.T.);
#4092=EDGE_CURVE('',#3365,#3367,#2087,.T.);
#4093=EDGE_CURVE('',#3368,#3366,#2088,.T.);
#4094=EDGE_CURVE('',#3367,#3368,#2089,.T.);
#4095=EDGE_CURVE('',#3367,#3369,#2090,.T.);
#4096=EDGE_CURVE('',#3370,#3368,#2091,.T.);
#4097=EDGE_CURVE('',#3369,#3370,#2092,.T.);
#4098=EDGE_CURVE('',#3369,#3371,#2093,.T.);
#4099=EDGE_CURVE('',#3372,#3370,#2094,.T.);
#4100=EDGE_CURVE('',#3371,#3372,#2095,.T.);
#4101=EDGE_CURVE('',#3371,#3373,#2096,.T.);
#4102=EDGE_CURVE('',#3374,#3372,#2097,.T.);
#4103=EDGE_CURVE('',#3373,#3374,#2098,.T.);
#4104=EDGE_CURVE('',#3373,#3375,#2099,.T.);
#4105=EDGE_CURVE('',#3376,#3374,#2100,.T.);
#4106=EDGE_CURVE('',#3375,#3376,#2101,.T.);
#4107=EDGE_CURVE('',#3375,#3377,#2102,.T.);
#4108=EDGE_CURVE('',#3378,#3376,#2103,.T.);
#4109=EDGE_CURVE('',#3377,#3378,#2104,.T.);
#4110=EDGE_CURVE('',#3377,#3379,#2105,.T.);
#4111=EDGE_CURVE('',#3380,#3378,#2106,.T.);
#4112=EDGE_CURVE('',#3379,#3380,#2107,.T.);
#4113=EDGE_CURVE('',#3379,#3381,#2108,.T.);
#4114=EDGE_CURVE('',#3382,#3380,#2109,.T.);
#4115=EDGE_CURVE('',#3381,#3382,#2110,.T.);
#4116=EDGE_CURVE('',#3381,#3383,#2111,.T.);
#4117=EDGE_CURVE('',#3384,#3382,#2112,.T.);
#4118=EDGE_CURVE('',#3383,#3384,#2113,.T.);
#4119=EDGE_CURVE('',#3383,#3385,#2114,.T.);
#4120=EDGE_CURVE('',#3386,#3384,#2115,.T.);
#4121=EDGE_CURVE('',#3385,#3386,#2116,.T.);
#4122=EDGE_CURVE('',#3385,#3387,#2117,.T.);
#4123=EDGE_CURVE('',#3388,#3386,#2118,.T.);
#4124=EDGE_CURVE('',#3387,#3388,#2119,.T.);
#4125=EDGE_CURVE('',#3387,#3389,#2120,.T.);
#4126=EDGE_CURVE('',#3390,#3388,#2121,.T.);
#4127=EDGE_CURVE('',#3389,#3390,#2122,.T.);
#4128=EDGE_CURVE('',#3389,#3391,#2123,.T.);
#4129=EDGE_CURVE('',#3392,#3390,#2124,.T.);
#4130=EDGE_CURVE('',#3391,#3392,#2125,.T.);
#4131=EDGE_CURVE('',#3391,#3393,#2126,.T.);
#4132=EDGE_CURVE('',#3394,#3392,#2127,.T.);
#4133=EDGE_CURVE('',#3393,#3394,#2128,.T.);
#4134=EDGE_CURVE('',#3393,#3395,#2129,.T.);
#4135=EDGE_CURVE('',#3396,#3394,#2130,.T.);
#4136=EDGE_CURVE('',#3395,#3396,#2131,.T.);
#4137=EDGE_CURVE('',#3395,#3301,#2132,.T.);
#4138=EDGE_CURVE('',#3303,#3396,#2133,.T.);
#4139=EDGE_CURVE('',#3397,#3397,#2910,.T.);
#4140=EDGE_CURVE('',#3397,#3398,#2134,.T.);
#4141=EDGE_CURVE('',#3398,#3398,#2911,.T.);
#4142=EDGE_CURVE('',#3399,#3400,#2135,.T.);
#4143=EDGE_CURVE('',#3399,#3400,#2912,.T.);
#4144=EDGE_CURVE('',#3401,#3399,#317,.T.);
#4145=EDGE_CURVE('',#3402,#3401,#2913,.T.);
#4146=EDGE_CURVE('',#3402,#3403,#2136,.T.);
#4147=EDGE_CURVE('',#3403,#3403,#2914,.T.);
#4148=EDGE_CURVE('',#3404,#3402,#2915,.T.);
#4149=EDGE_CURVE('',#3400,#3404,#318,.T.);
#4150=EDGE_CURVE('',#3404,#3401,#2137,.T.);
#4151=EDGE_CURVE('',#3405,#3406,#2916,.T.);
#4152=EDGE_CURVE('',#3405,#3407,#2138,.T.);
#4153=EDGE_CURVE('',#3407,#3408,#2139,.T.);
#4154=EDGE_CURVE('',#3408,#3409,#2140,.T.);
#4155=EDGE_CURVE('',#3406,#3409,#2917,.T.);
#4156=EDGE_CURVE('',#3410,#3410,#2918,.T.);
#4157=EDGE_CURVE('',#3409,#3411,#2141,.T.);
#4158=EDGE_CURVE('',#3408,#3412,#2142,.T.);
#4159=EDGE_CURVE('',#3411,#3412,#2143,.T.);
#4160=EDGE_CURVE('',#3411,#3413,#2919,.T.);
#4161=EDGE_CURVE('',#3412,#3414,#2144,.T.);
#4162=EDGE_CURVE('',#3414,#3413,#2145,.T.);
#4163=EDGE_CURVE('',#3413,#3405,#2146,.T.);
#4164=EDGE_CURVE('',#3407,#3414,#2147,.T.);
#4165=EDGE_CURVE('',#3415,#3415,#2920,.T.);
#4166=EDGE_CURVE('',#3415,#3406,#2148,.T.);
#4167=EDGE_CURVE('',#3416,#3416,#2921,.T.);
#4168=EDGE_CURVE('',#3416,#3410,#2149,.T.);
#4169=EDGE_CURVE('',#3417,#3417,#2922,.T.);
#4170=EDGE_CURVE('',#3417,#3418,#2150,.T.);
#4171=EDGE_CURVE('',#3418,#3418,#2923,.T.);
#4172=EDGE_CURVE('',#3419,#3419,#2924,.T.);
#4173=EDGE_CURVE('',#3419,#3420,#2151,.T.);
#4174=EDGE_CURVE('',#3420,#3420,#2925,.T.);
#4175=EDGE_CURVE('',#3421,#3422,#2152,.T.);
#4176=EDGE_CURVE('',#3421,#3423,#2153,.T.);
#4177=EDGE_CURVE('',#3423,#3424,#2154,.T.);
#4178=EDGE_CURVE('',#3422,#3424,#2155,.T.);
#4179=EDGE_CURVE('',#3425,#3421,#2156,.T.);
#4180=EDGE_CURVE('',#3425,#3426,#2157,.T.);
#4181=EDGE_CURVE('',#3426,#3423,#2158,.T.);
#4182=EDGE_CURVE('',#3427,#3425,#2159,.T.);
#4183=EDGE_CURVE('',#3427,#3428,#2160,.T.);
#4184=EDGE_CURVE('',#3428,#3426,#2161,.T.);
#4185=EDGE_CURVE('',#3429,#3427,#2162,.T.);
#4186=EDGE_CURVE('',#3429,#3430,#2163,.T.);
#4187=EDGE_CURVE('',#3430,#3428,#2164,.T.);
#4188=EDGE_CURVE('',#3431,#3429,#2165,.T.);
#4189=EDGE_CURVE('',#3431,#3432,#2166,.T.);
#4190=EDGE_CURVE('',#3432,#3430,#2167,.T.);
#4191=EDGE_CURVE('',#3422,#3431,#2168,.T.);
#4192=EDGE_CURVE('',#3424,#3432,#2169,.T.);
#4193=EDGE_CURVE('',#3433,#3433,#2926,.T.);
#4194=EDGE_CURVE('',#3434,#3434,#2927,.T.);
#4195=EDGE_CURVE('',#3434,#3433,#2170,.T.);
#4196=EDGE_CURVE('',#3435,#3435,#2928,.F.);
#4197=EDGE_CURVE('',#3435,#3434,#2171,.T.);
#4198=EDGE_CURVE('',#3436,#3436,#2929,.T.);
#4199=EDGE_CURVE('',#3436,#3435,#2172,.T.);
#4200=EDGE_CURVE('',#3437,#3437,#2930,.T.);
#4201=EDGE_CURVE('',#3438,#3438,#2931,.T.);
#4202=EDGE_CURVE('',#3438,#3437,#2173,.T.);
#4203=EDGE_CURVE('',#3439,#3439,#2932,.T.);
#4204=EDGE_CURVE('',#3439,#3438,#2174,.T.);
#4205=EDGE_CURVE('',#3440,#3440,#2933,.T.);
#4206=EDGE_CURVE('',#3440,#3439,#2175,.T.);
#4207=EDGE_CURVE('',#3441,#3441,#2934,.T.);
#4208=EDGE_CURVE('',#3442,#3442,#2935,.F.);
#4209=EDGE_CURVE('',#3442,#3441,#2176,.T.);
#4210=EDGE_CURVE('',#3443,#3443,#2936,.F.);
#4211=EDGE_CURVE('',#3443,#3442,#2177,.T.);
#4212=EDGE_CURVE('',#3444,#3444,#2937,.T.);
#4213=EDGE_CURVE('',#3444,#3443,#2178,.T.);
#4214=EDGE_CURVE('',#3445,#3446,#2179,.T.);
#4215=EDGE_CURVE('',#3446,#3447,#2180,.T.);
#4216=EDGE_CURVE('',#3447,#3448,#2181,.T.);
#4217=EDGE_CURVE('',#3445,#3448,#2182,.T.);
#4218=EDGE_CURVE('',#3446,#3449,#2183,.T.);
#4219=EDGE_CURVE('',#3449,#3450,#2184,.T.);
#4220=EDGE_CURVE('',#3450,#3447,#2185,.T.);
#4221=EDGE_CURVE('',#3449,#3451,#2186,.T.);
#4222=EDGE_CURVE('',#3451,#3452,#2187,.T.);
#4223=EDGE_CURVE('',#3452,#3450,#2188,.T.);
#4224=EDGE_CURVE('',#3451,#3453,#2189,.T.);
#4225=EDGE_CURVE('',#3453,#3454,#2190,.T.);
#4226=EDGE_CURVE('',#3454,#3452,#2191,.T.);
#4227=EDGE_CURVE('',#3453,#3455,#2192,.T.);
#4228=EDGE_CURVE('',#3455,#3456,#2193,.T.);
#4229=EDGE_CURVE('',#3456,#3454,#2194,.T.);
#4230=EDGE_CURVE('',#3455,#3445,#2195,.T.);
#4231=EDGE_CURVE('',#3448,#3456,#2196,.T.);
#4232=EDGE_CURVE('',#3457,#3457,#2938,.T.);
#4233=EDGE_CURVE('',#3457,#3458,#2197,.T.);
#4234=EDGE_CURVE('',#3458,#3458,#2939,.T.);
#4235=EDGE_CURVE('',#3459,#3460,#2198,.T.);
#4236=EDGE_CURVE('',#3459,#3461,#2940,.T.);
#4237=EDGE_CURVE('',#3462,#3461,#2199,.T.);
#4238=EDGE_CURVE('',#3460,#3462,#2941,.T.);
#4239=EDGE_CURVE('',#3463,#3460,#2200,.T.);
#4240=EDGE_CURVE('',#3464,#3463,#2201,.T.);
#4241=EDGE_CURVE('',#3459,#3464,#2202,.T.);
#4242=EDGE_CURVE('',#3462,#3465,#2203,.T.);
#4243=EDGE_CURVE('',#3465,#3463,#2204,.T.);
#4244=EDGE_CURVE('',#3464,#3466,#2205,.T.);
#4245=EDGE_CURVE('',#3466,#3465,#2206,.T.);
#4246=EDGE_CURVE('',#3466,#3461,#2207,.T.);
#4247=ORIENTED_EDGE('',*,*,#3467,.F.);
#4248=ORIENTED_EDGE('',*,*,#3468,.T.);
#4249=ORIENTED_EDGE('',*,*,#3469,.F.);
#4250=ORIENTED_EDGE('',*,*,#3468,.F.);
#4251=ORIENTED_EDGE('',*,*,#3470,.F.);
#4252=ORIENTED_EDGE('',*,*,#3471,.T.);
#4253=ORIENTED_EDGE('',*,*,#3472,.F.);
#4254=ORIENTED_EDGE('',*,*,#3471,.F.);
#4255=ORIENTED_EDGE('',*,*,#3473,.F.);
#4256=ORIENTED_EDGE('',*,*,#3474,.T.);
#4257=ORIENTED_EDGE('',*,*,#3475,.F.);
#4258=ORIENTED_EDGE('',*,*,#3474,.F.);
#4259=ORIENTED_EDGE('',*,*,#3476,.F.);
#4260=ORIENTED_EDGE('',*,*,#3477,.T.);
#4261=ORIENTED_EDGE('',*,*,#3478,.F.);
#4262=ORIENTED_EDGE('',*,*,#3477,.F.);
#4263=ORIENTED_EDGE('',*,*,#3479,.F.);
#4264=ORIENTED_EDGE('',*,*,#3480,.T.);
#4265=ORIENTED_EDGE('',*,*,#3481,.F.);
#4266=ORIENTED_EDGE('',*,*,#3480,.F.);
#4267=ORIENTED_EDGE('',*,*,#3482,.F.);
#4268=ORIENTED_EDGE('',*,*,#3483,.T.);
#4269=ORIENTED_EDGE('',*,*,#3484,.F.);
#4270=ORIENTED_EDGE('',*,*,#3483,.F.);
#4271=ORIENTED_EDGE('',*,*,#3485,.F.);
#4272=ORIENTED_EDGE('',*,*,#3486,.T.);
#4273=ORIENTED_EDGE('',*,*,#3487,.F.);
#4274=ORIENTED_EDGE('',*,*,#3486,.F.);
#4275=ORIENTED_EDGE('',*,*,#3488,.F.);
#4276=ORIENTED_EDGE('',*,*,#3489,.T.);
#4277=ORIENTED_EDGE('',*,*,#3490,.F.);
#4278=ORIENTED_EDGE('',*,*,#3489,.F.);
#4279=ORIENTED_EDGE('',*,*,#3491,.F.);
#4280=ORIENTED_EDGE('',*,*,#3492,.T.);
#4281=ORIENTED_EDGE('',*,*,#3493,.F.);
#4282=ORIENTED_EDGE('',*,*,#3492,.F.);
#4283=ORIENTED_EDGE('',*,*,#3494,.F.);
#4284=ORIENTED_EDGE('',*,*,#3495,.T.);
#4285=ORIENTED_EDGE('',*,*,#3496,.F.);
#4286=ORIENTED_EDGE('',*,*,#3495,.F.);
#4287=ORIENTED_EDGE('',*,*,#3497,.T.);
#4288=ORIENTED_EDGE('',*,*,#3498,.T.);
#4289=ORIENTED_EDGE('',*,*,#3499,.F.);
#4290=ORIENTED_EDGE('',*,*,#3500,.F.);
#4291=ORIENTED_EDGE('',*,*,#3501,.T.);
#4292=ORIENTED_EDGE('',*,*,#3500,.T.);
#4293=ORIENTED_EDGE('',*,*,#3502,.F.);
#4294=ORIENTED_EDGE('',*,*,#3503,.F.);
#4295=ORIENTED_EDGE('',*,*,#3504,.T.);
#4296=ORIENTED_EDGE('',*,*,#3503,.T.);
#4297=ORIENTED_EDGE('',*,*,#3505,.F.);
#4298=ORIENTED_EDGE('',*,*,#3506,.F.);
#4299=ORIENTED_EDGE('',*,*,#3507,.T.);
#4300=ORIENTED_EDGE('',*,*,#3506,.T.);
#4301=ORIENTED_EDGE('',*,*,#3508,.F.);
#4302=ORIENTED_EDGE('',*,*,#3498,.F.);
#4303=ORIENTED_EDGE('',*,*,#3508,.T.);
#4304=ORIENTED_EDGE('',*,*,#3505,.T.);
#4305=ORIENTED_EDGE('',*,*,#3502,.T.);
#4306=ORIENTED_EDGE('',*,*,#3499,.T.);
#4307=ORIENTED_EDGE('',*,*,#3472,.T.);
#4308=ORIENTED_EDGE('',*,*,#3496,.T.);
#4309=ORIENTED_EDGE('',*,*,#3493,.T.);
#4310=ORIENTED_EDGE('',*,*,#3490,.T.);
#4311=ORIENTED_EDGE('',*,*,#3487,.T.);
#4312=ORIENTED_EDGE('',*,*,#3484,.T.);
#4313=ORIENTED_EDGE('',*,*,#3481,.T.);
#4314=ORIENTED_EDGE('',*,*,#3478,.T.);
#4315=ORIENTED_EDGE('',*,*,#3475,.T.);
#4316=ORIENTED_EDGE('',*,*,#3469,.T.);
#4317=ORIENTED_EDGE('',*,*,#3507,.F.);
#4318=ORIENTED_EDGE('',*,*,#3497,.F.);
#4319=ORIENTED_EDGE('',*,*,#3501,.F.);
#4320=ORIENTED_EDGE('',*,*,#3504,.F.);
#4321=ORIENTED_EDGE('',*,*,#3470,.T.);
#4322=ORIENTED_EDGE('',*,*,#3494,.T.);
#4323=ORIENTED_EDGE('',*,*,#3491,.T.);
#4324=ORIENTED_EDGE('',*,*,#3488,.T.);
#4325=ORIENTED_EDGE('',*,*,#3485,.T.);
#4326=ORIENTED_EDGE('',*,*,#3482,.T.);
#4327=ORIENTED_EDGE('',*,*,#3479,.T.);
#4328=ORIENTED_EDGE('',*,*,#3476,.T.);
#4329=ORIENTED_EDGE('',*,*,#3473,.T.);
#4330=ORIENTED_EDGE('',*,*,#3467,.T.);
#4331=ORIENTED_EDGE('',*,*,#3509,.T.);
#4332=ORIENTED_EDGE('',*,*,#3510,.T.);
#4333=ORIENTED_EDGE('',*,*,#3511,.F.);
#4334=ORIENTED_EDGE('',*,*,#3512,.F.);
#4335=ORIENTED_EDGE('',*,*,#3513,.T.);
#4336=ORIENTED_EDGE('',*,*,#3512,.T.);
#4337=ORIENTED_EDGE('',*,*,#3514,.F.);
#4338=ORIENTED_EDGE('',*,*,#3515,.F.);
#4339=ORIENTED_EDGE('',*,*,#3516,.T.);
#4340=ORIENTED_EDGE('',*,*,#3515,.T.);
#4341=ORIENTED_EDGE('',*,*,#3517,.F.);
#4342=ORIENTED_EDGE('',*,*,#3518,.F.);
#4343=ORIENTED_EDGE('',*,*,#3519,.T.);
#4344=ORIENTED_EDGE('',*,*,#3518,.T.);
#4345=ORIENTED_EDGE('',*,*,#3520,.F.);
#4346=ORIENTED_EDGE('',*,*,#3510,.F.);
#4347=ORIENTED_EDGE('',*,*,#3520,.T.);
#4348=ORIENTED_EDGE('',*,*,#3517,.T.);
#4349=ORIENTED_EDGE('',*,*,#3514,.T.);
#4350=ORIENTED_EDGE('',*,*,#3511,.T.);
#4351=ORIENTED_EDGE('',*,*,#3519,.F.);
#4352=ORIENTED_EDGE('',*,*,#3509,.F.);
#4353=ORIENTED_EDGE('',*,*,#3513,.F.);
#4354=ORIENTED_EDGE('',*,*,#3516,.F.);
#4355=ORIENTED_EDGE('',*,*,#3521,.T.);
#4356=ORIENTED_EDGE('',*,*,#3522,.T.);
#4357=ORIENTED_EDGE('',*,*,#3523,.F.);
#4358=ORIENTED_EDGE('',*,*,#3524,.F.);
#4359=ORIENTED_EDGE('',*,*,#3525,.T.);
#4360=ORIENTED_EDGE('',*,*,#3524,.T.);
#4361=ORIENTED_EDGE('',*,*,#3526,.F.);
#4362=ORIENTED_EDGE('',*,*,#3527,.F.);
#4363=ORIENTED_EDGE('',*,*,#3528,.T.);
#4364=ORIENTED_EDGE('',*,*,#3527,.T.);
#4365=ORIENTED_EDGE('',*,*,#3529,.F.);
#4366=ORIENTED_EDGE('',*,*,#3530,.F.);
#4367=ORIENTED_EDGE('',*,*,#3531,.T.);
#4368=ORIENTED_EDGE('',*,*,#3530,.T.);
#4369=ORIENTED_EDGE('',*,*,#3532,.F.);
#4370=ORIENTED_EDGE('',*,*,#3522,.F.);
#4371=ORIENTED_EDGE('',*,*,#3532,.T.);
#4372=ORIENTED_EDGE('',*,*,#3529,.T.);
#4373=ORIENTED_EDGE('',*,*,#3526,.T.);
#4374=ORIENTED_EDGE('',*,*,#3523,.T.);
#4375=ORIENTED_EDGE('',*,*,#3531,.F.);
#4376=ORIENTED_EDGE('',*,*,#3521,.F.);
#4377=ORIENTED_EDGE('',*,*,#3525,.F.);
#4378=ORIENTED_EDGE('',*,*,#3528,.F.);
#4379=ORIENTED_EDGE('',*,*,#3533,.F.);
#4380=ORIENTED_EDGE('',*,*,#3534,.T.);
#4381=ORIENTED_EDGE('',*,*,#3535,.F.);
#4382=ORIENTED_EDGE('',*,*,#3534,.F.);
#4383=ORIENTED_EDGE('',*,*,#3533,.T.);
#4384=ORIENTED_EDGE('',*,*,#3536,.F.);
#4385=ORIENTED_EDGE('',*,*,#3537,.F.);
#4386=ORIENTED_EDGE('',*,*,#3538,.T.);
#4387=ORIENTED_EDGE('',*,*,#3539,.F.);
#4388=ORIENTED_EDGE('',*,*,#3538,.F.);
#4389=ORIENTED_EDGE('',*,*,#3537,.T.);
#4390=ORIENTED_EDGE('',*,*,#3540,.F.);
#4391=ORIENTED_EDGE('',*,*,#3541,.F.);
#4392=ORIENTED_EDGE('',*,*,#3542,.T.);
#4393=ORIENTED_EDGE('',*,*,#3536,.T.);
#4394=ORIENTED_EDGE('',*,*,#3542,.F.);
#4395=ORIENTED_EDGE('',*,*,#3543,.F.);
#4396=ORIENTED_EDGE('',*,*,#3544,.T.);
#4397=ORIENTED_EDGE('',*,*,#3540,.T.);
#4398=ORIENTED_EDGE('',*,*,#3544,.F.);
#4399=ORIENTED_EDGE('',*,*,#3545,.F.);
#4400=ORIENTED_EDGE('',*,*,#3546,.T.);
#4401=ORIENTED_EDGE('',*,*,#3547,.F.);
#4402=ORIENTED_EDGE('',*,*,#3546,.F.);
#4403=ORIENTED_EDGE('',*,*,#3545,.T.);
#4404=ORIENTED_EDGE('',*,*,#3548,.F.);
#4405=ORIENTED_EDGE('',*,*,#3549,.F.);
#4406=ORIENTED_EDGE('',*,*,#3550,.T.);
#4407=ORIENTED_EDGE('',*,*,#3551,.F.);
#4408=ORIENTED_EDGE('',*,*,#3550,.F.);
#4409=ORIENTED_EDGE('',*,*,#3549,.T.);
#4410=ORIENTED_EDGE('',*,*,#3552,.F.);
#4411=ORIENTED_EDGE('',*,*,#3553,.F.);
#4412=ORIENTED_EDGE('',*,*,#3554,.T.);
#4413=ORIENTED_EDGE('',*,*,#3548,.T.);
#4414=ORIENTED_EDGE('',*,*,#3554,.F.);
#4415=ORIENTED_EDGE('',*,*,#3555,.F.);
#4416=ORIENTED_EDGE('',*,*,#3556,.T.);
#4417=ORIENTED_EDGE('',*,*,#3552,.T.);
#4418=ORIENTED_EDGE('',*,*,#3556,.F.);
#4419=ORIENTED_EDGE('',*,*,#3557,.F.);
#4420=ORIENTED_EDGE('',*,*,#3558,.T.);
#4421=ORIENTED_EDGE('',*,*,#3559,.F.);
#4422=ORIENTED_EDGE('',*,*,#3558,.F.);
#4423=ORIENTED_EDGE('',*,*,#3560,.F.);
#4424=ORIENTED_EDGE('',*,*,#3561,.T.);
#4425=ORIENTED_EDGE('',*,*,#3562,.F.);
#4426=ORIENTED_EDGE('',*,*,#3561,.F.);
#4427=ORIENTED_EDGE('',*,*,#3563,.T.);
#4428=ORIENTED_EDGE('',*,*,#3564,.T.);
#4429=ORIENTED_EDGE('',*,*,#3565,.F.);
#4430=ORIENTED_EDGE('',*,*,#3566,.F.);
#4431=ORIENTED_EDGE('',*,*,#3567,.T.);
#4432=ORIENTED_EDGE('',*,*,#3566,.T.);
#4433=ORIENTED_EDGE('',*,*,#3568,.F.);
#4434=ORIENTED_EDGE('',*,*,#3569,.F.);
#4435=ORIENTED_EDGE('',*,*,#3570,.T.);
#4436=ORIENTED_EDGE('',*,*,#3569,.T.);
#4437=ORIENTED_EDGE('',*,*,#3571,.F.);
#4438=ORIENTED_EDGE('',*,*,#3572,.F.);
#4439=ORIENTED_EDGE('',*,*,#3573,.T.);
#4440=ORIENTED_EDGE('',*,*,#3572,.T.);
#4441=ORIENTED_EDGE('',*,*,#3574,.F.);
#4442=ORIENTED_EDGE('',*,*,#3564,.F.);
#4443=ORIENTED_EDGE('',*,*,#3574,.T.);
#4444=ORIENTED_EDGE('',*,*,#3571,.T.);
#4445=ORIENTED_EDGE('',*,*,#3568,.T.);
#4446=ORIENTED_EDGE('',*,*,#3565,.T.);
#4447=ORIENTED_EDGE('',*,*,#3562,.T.);
#4448=ORIENTED_EDGE('',*,*,#3559,.T.);
#4449=ORIENTED_EDGE('',*,*,#3551,.T.);
#4450=ORIENTED_EDGE('',*,*,#3547,.T.);
#4451=ORIENTED_EDGE('',*,*,#3539,.T.);
#4452=ORIENTED_EDGE('',*,*,#3535,.T.);
#4453=ORIENTED_EDGE('',*,*,#3573,.F.);
#4454=ORIENTED_EDGE('',*,*,#3563,.F.);
#4455=ORIENTED_EDGE('',*,*,#3567,.F.);
#4456=ORIENTED_EDGE('',*,*,#3570,.F.);
#4457=ORIENTED_EDGE('',*,*,#3541,.T.);
#4458=ORIENTED_EDGE('',*,*,#3543,.T.);
#4459=ORIENTED_EDGE('',*,*,#3553,.T.);
#4460=ORIENTED_EDGE('',*,*,#3555,.T.);
#4461=ORIENTED_EDGE('',*,*,#3557,.T.);
#4462=ORIENTED_EDGE('',*,*,#3560,.T.);
#4463=ORIENTED_EDGE('',*,*,#3575,.F.);
#4464=ORIENTED_EDGE('',*,*,#3576,.T.);
#4465=ORIENTED_EDGE('',*,*,#3577,.T.);
#4466=ORIENTED_EDGE('',*,*,#3576,.F.);
#4467=ORIENTED_EDGE('',*,*,#3578,.F.);
#4468=ORIENTED_EDGE('',*,*,#3579,.T.);
#4469=ORIENTED_EDGE('',*,*,#3580,.T.);
#4470=ORIENTED_EDGE('',*,*,#3579,.F.);
#4471=ORIENTED_EDGE('',*,*,#3578,.T.);
#4472=ORIENTED_EDGE('',*,*,#3575,.T.);
#4473=ORIENTED_EDGE('',*,*,#3580,.F.);
#4474=ORIENTED_EDGE('',*,*,#3577,.F.);
#4475=ORIENTED_EDGE('',*,*,#3581,.F.);
#4476=ORIENTED_EDGE('',*,*,#3582,.T.);
#4477=ORIENTED_EDGE('',*,*,#3583,.T.);
#4478=ORIENTED_EDGE('',*,*,#3582,.F.);
#4479=ORIENTED_EDGE('',*,*,#3584,.F.);
#4480=ORIENTED_EDGE('',*,*,#3585,.T.);
#4481=ORIENTED_EDGE('',*,*,#3586,.T.);
#4482=ORIENTED_EDGE('',*,*,#3585,.F.);
#4483=ORIENTED_EDGE('',*,*,#3584,.T.);
#4484=ORIENTED_EDGE('',*,*,#3581,.T.);
#4485=ORIENTED_EDGE('',*,*,#3586,.F.);
#4486=ORIENTED_EDGE('',*,*,#3583,.F.);
#4487=ORIENTED_EDGE('',*,*,#3587,.F.);
#4488=ORIENTED_EDGE('',*,*,#3588,.T.);
#4489=ORIENTED_EDGE('',*,*,#3589,.F.);
#4490=ORIENTED_EDGE('',*,*,#3588,.F.);
#4491=ORIENTED_EDGE('',*,*,#3587,.T.);
#4492=ORIENTED_EDGE('',*,*,#3590,.F.);
#4493=ORIENTED_EDGE('',*,*,#3591,.F.);
#4494=ORIENTED_EDGE('',*,*,#3592,.T.);
#4495=ORIENTED_EDGE('',*,*,#3593,.F.);
#4496=ORIENTED_EDGE('',*,*,#3592,.F.);
#4497=ORIENTED_EDGE('',*,*,#3591,.T.);
#4498=ORIENTED_EDGE('',*,*,#3594,.F.);
#4499=ORIENTED_EDGE('',*,*,#3595,.F.);
#4500=ORIENTED_EDGE('',*,*,#3596,.T.);
#4501=ORIENTED_EDGE('',*,*,#3590,.T.);
#4502=ORIENTED_EDGE('',*,*,#3596,.F.);
#4503=ORIENTED_EDGE('',*,*,#3597,.F.);
#4504=ORIENTED_EDGE('',*,*,#3598,.T.);
#4505=ORIENTED_EDGE('',*,*,#3594,.T.);
#4506=ORIENTED_EDGE('',*,*,#3598,.F.);
#4507=ORIENTED_EDGE('',*,*,#3599,.F.);
#4508=ORIENTED_EDGE('',*,*,#3600,.T.);
#4509=ORIENTED_EDGE('',*,*,#3601,.F.);
#4510=ORIENTED_EDGE('',*,*,#3600,.F.);
#4511=ORIENTED_EDGE('',*,*,#3599,.T.);
#4512=ORIENTED_EDGE('',*,*,#3602,.F.);
#4513=ORIENTED_EDGE('',*,*,#3603,.F.);
#4514=ORIENTED_EDGE('',*,*,#3604,.T.);
#4515=ORIENTED_EDGE('',*,*,#3605,.F.);
#4516=ORIENTED_EDGE('',*,*,#3604,.F.);
#4517=ORIENTED_EDGE('',*,*,#3603,.T.);
#4518=ORIENTED_EDGE('',*,*,#3606,.F.);
#4519=ORIENTED_EDGE('',*,*,#3607,.F.);
#4520=ORIENTED_EDGE('',*,*,#3608,.T.);
#4521=ORIENTED_EDGE('',*,*,#3602,.T.);
#4522=ORIENTED_EDGE('',*,*,#3608,.F.);
#4523=ORIENTED_EDGE('',*,*,#3609,.F.);
#4524=ORIENTED_EDGE('',*,*,#3610,.T.);
#4525=ORIENTED_EDGE('',*,*,#3606,.T.);
#4526=ORIENTED_EDGE('',*,*,#3610,.F.);
#4527=ORIENTED_EDGE('',*,*,#3611,.F.);
#4528=ORIENTED_EDGE('',*,*,#3612,.T.);
#4529=ORIENTED_EDGE('',*,*,#3613,.F.);
#4530=ORIENTED_EDGE('',*,*,#3612,.F.);
#4531=ORIENTED_EDGE('',*,*,#3614,.F.);
#4532=ORIENTED_EDGE('',*,*,#3615,.T.);
#4533=ORIENTED_EDGE('',*,*,#3616,.F.);
#4534=ORIENTED_EDGE('',*,*,#3615,.F.);
#4535=ORIENTED_EDGE('',*,*,#3617,.T.);
#4536=ORIENTED_EDGE('',*,*,#3618,.T.);
#4537=ORIENTED_EDGE('',*,*,#3619,.F.);
#4538=ORIENTED_EDGE('',*,*,#3620,.F.);
#4539=ORIENTED_EDGE('',*,*,#3621,.T.);
#4540=ORIENTED_EDGE('',*,*,#3620,.T.);
#4541=ORIENTED_EDGE('',*,*,#3622,.F.);
#4542=ORIENTED_EDGE('',*,*,#3623,.F.);
#4543=ORIENTED_EDGE('',*,*,#3624,.T.);
#4544=ORIENTED_EDGE('',*,*,#3623,.T.);
#4545=ORIENTED_EDGE('',*,*,#3625,.F.);
#4546=ORIENTED_EDGE('',*,*,#3626,.F.);
#4547=ORIENTED_EDGE('',*,*,#3627,.T.);
#4548=ORIENTED_EDGE('',*,*,#3626,.T.);
#4549=ORIENTED_EDGE('',*,*,#3628,.F.);
#4550=ORIENTED_EDGE('',*,*,#3618,.F.);
#4551=ORIENTED_EDGE('',*,*,#3628,.T.);
#4552=ORIENTED_EDGE('',*,*,#3625,.T.);
#4553=ORIENTED_EDGE('',*,*,#3622,.T.);
#4554=ORIENTED_EDGE('',*,*,#3619,.T.);
#4555=ORIENTED_EDGE('',*,*,#3616,.T.);
#4556=ORIENTED_EDGE('',*,*,#3613,.T.);
#4557=ORIENTED_EDGE('',*,*,#3605,.T.);
#4558=ORIENTED_EDGE('',*,*,#3601,.T.);
#4559=ORIENTED_EDGE('',*,*,#3593,.T.);
#4560=ORIENTED_EDGE('',*,*,#3589,.T.);
#4561=ORIENTED_EDGE('',*,*,#3627,.F.);
#4562=ORIENTED_EDGE('',*,*,#3617,.F.);
#4563=ORIENTED_EDGE('',*,*,#3621,.F.);
#4564=ORIENTED_EDGE('',*,*,#3624,.F.);
#4565=ORIENTED_EDGE('',*,*,#3595,.T.);
#4566=ORIENTED_EDGE('',*,*,#3597,.T.);
#4567=ORIENTED_EDGE('',*,*,#3607,.T.);
#4568=ORIENTED_EDGE('',*,*,#3609,.T.);
#4569=ORIENTED_EDGE('',*,*,#3611,.T.);
#4570=ORIENTED_EDGE('',*,*,#3614,.T.);
#4571=ORIENTED_EDGE('',*,*,#3629,.F.);
#4572=ORIENTED_EDGE('',*,*,#3630,.T.);
#4573=ORIENTED_EDGE('',*,*,#3631,.T.);
#4574=ORIENTED_EDGE('',*,*,#3630,.F.);
#4575=ORIENTED_EDGE('',*,*,#3632,.F.);
#4576=ORIENTED_EDGE('',*,*,#3633,.T.);
#4577=ORIENTED_EDGE('',*,*,#3634,.T.);
#4578=ORIENTED_EDGE('',*,*,#3633,.F.);
#4579=ORIENTED_EDGE('',*,*,#3632,.T.);
#4580=ORIENTED_EDGE('',*,*,#3629,.T.);
#4581=ORIENTED_EDGE('',*,*,#3634,.F.);
#4582=ORIENTED_EDGE('',*,*,#3631,.F.);
#4583=ORIENTED_EDGE('',*,*,#3635,.F.);
#4584=ORIENTED_EDGE('',*,*,#3636,.T.);
#4585=ORIENTED_EDGE('',*,*,#3637,.T.);
#4586=ORIENTED_EDGE('',*,*,#3636,.F.);
#4587=ORIENTED_EDGE('',*,*,#3638,.F.);
#4588=ORIENTED_EDGE('',*,*,#3639,.T.);
#4589=ORIENTED_EDGE('',*,*,#3640,.T.);
#4590=ORIENTED_EDGE('',*,*,#3639,.F.);
#4591=ORIENTED_EDGE('',*,*,#3638,.T.);
#4592=ORIENTED_EDGE('',*,*,#3635,.T.);
#4593=ORIENTED_EDGE('',*,*,#3640,.F.);
#4594=ORIENTED_EDGE('',*,*,#3637,.F.);
#4595=ORIENTED_EDGE('',*,*,#3641,.F.);
#4596=ORIENTED_EDGE('',*,*,#3642,.T.);
#4597=ORIENTED_EDGE('',*,*,#3643,.F.);
#4598=ORIENTED_EDGE('',*,*,#3642,.F.);
#4599=ORIENTED_EDGE('',*,*,#3644,.F.);
#4600=ORIENTED_EDGE('',*,*,#3645,.T.);
#4601=ORIENTED_EDGE('',*,*,#3646,.F.);
#4602=ORIENTED_EDGE('',*,*,#3645,.F.);
#4603=ORIENTED_EDGE('',*,*,#3647,.F.);
#4604=ORIENTED_EDGE('',*,*,#3648,.T.);
#4605=ORIENTED_EDGE('',*,*,#3649,.F.);
#4606=ORIENTED_EDGE('',*,*,#3648,.F.);
#4607=ORIENTED_EDGE('',*,*,#3650,.F.);
#4608=ORIENTED_EDGE('',*,*,#3651,.T.);
#4609=ORIENTED_EDGE('',*,*,#3652,.F.);
#4610=ORIENTED_EDGE('',*,*,#3653,.F.);
#4611=ORIENTED_EDGE('',*,*,#3643,.T.);
#4612=ORIENTED_EDGE('',*,*,#3646,.T.);
#4613=ORIENTED_EDGE('',*,*,#3654,.F.);
#4614=ORIENTED_EDGE('',*,*,#3655,.F.);
#4615=ORIENTED_EDGE('',*,*,#3656,.F.);
#4616=ORIENTED_EDGE('',*,*,#3657,.F.);
#4617=ORIENTED_EDGE('',*,*,#3658,.F.);
#4618=ORIENTED_EDGE('',*,*,#3653,.T.);
#4619=ORIENTED_EDGE('',*,*,#3659,.F.);
#4620=ORIENTED_EDGE('',*,*,#3660,.F.);
#4621=ORIENTED_EDGE('',*,*,#3661,.F.);
#4622=ORIENTED_EDGE('',*,*,#3662,.T.);
#4623=ORIENTED_EDGE('',*,*,#3663,.F.);
#4624=ORIENTED_EDGE('',*,*,#3651,.F.);
#4625=ORIENTED_EDGE('',*,*,#3652,.T.);
#4626=ORIENTED_EDGE('',*,*,#3663,.T.);
#4627=ORIENTED_EDGE('',*,*,#3664,.T.);
#4628=ORIENTED_EDGE('',*,*,#3659,.T.);
#4629=ORIENTED_EDGE('',*,*,#3650,.T.);
#4630=ORIENTED_EDGE('',*,*,#3658,.T.);
#4631=ORIENTED_EDGE('',*,*,#3665,.T.);
#4632=ORIENTED_EDGE('',*,*,#3661,.T.);
#4633=ORIENTED_EDGE('',*,*,#3656,.T.);
#4634=ORIENTED_EDGE('',*,*,#3666,.T.);
#4635=ORIENTED_EDGE('',*,*,#3667,.F.);
#4636=ORIENTED_EDGE('',*,*,#3668,.F.);
#4637=ORIENTED_EDGE('',*,*,#3647,.T.);
#4638=ORIENTED_EDGE('',*,*,#3655,.T.);
#4639=ORIENTED_EDGE('',*,*,#3669,.T.);
#4640=ORIENTED_EDGE('',*,*,#3670,.F.);
#4641=ORIENTED_EDGE('',*,*,#3666,.F.);
#4642=ORIENTED_EDGE('',*,*,#3654,.T.);
#4643=ORIENTED_EDGE('',*,*,#3671,.T.);
#4644=ORIENTED_EDGE('',*,*,#3672,.F.);
#4645=ORIENTED_EDGE('',*,*,#3669,.F.);
#4646=ORIENTED_EDGE('',*,*,#3649,.T.);
#4647=ORIENTED_EDGE('',*,*,#3657,.T.);
#4648=ORIENTED_EDGE('',*,*,#3668,.T.);
#4649=ORIENTED_EDGE('',*,*,#3673,.F.);
#4650=ORIENTED_EDGE('',*,*,#3671,.F.);
#4651=ORIENTED_EDGE('',*,*,#3673,.T.);
#4652=ORIENTED_EDGE('',*,*,#3667,.T.);
#4653=ORIENTED_EDGE('',*,*,#3670,.T.);
#4654=ORIENTED_EDGE('',*,*,#3672,.T.);
#4655=ORIENTED_EDGE('',*,*,#3665,.F.);
#4656=ORIENTED_EDGE('',*,*,#3660,.T.);
#4657=ORIENTED_EDGE('',*,*,#3664,.F.);
#4658=ORIENTED_EDGE('',*,*,#3662,.F.);
#4659=ORIENTED_EDGE('',*,*,#3641,.T.);
#4660=ORIENTED_EDGE('',*,*,#3644,.T.);
#4661=ORIENTED_EDGE('',*,*,#3674,.F.);
#4662=ORIENTED_EDGE('',*,*,#3675,.T.);
#4663=ORIENTED_EDGE('',*,*,#3676,.F.);
#4664=ORIENTED_EDGE('',*,*,#3675,.F.);
#4665=ORIENTED_EDGE('',*,*,#3674,.T.);
#4666=ORIENTED_EDGE('',*,*,#3677,.T.);
#4667=ORIENTED_EDGE('',*,*,#3678,.F.);
#4668=ORIENTED_EDGE('',*,*,#3677,.F.);
#4669=ORIENTED_EDGE('',*,*,#3679,.T.);
#4670=ORIENTED_EDGE('',*,*,#3680,.T.);
#4671=ORIENTED_EDGE('',*,*,#3679,.F.);
#4672=ORIENTED_EDGE('',*,*,#3680,.F.);
#4673=ORIENTED_EDGE('',*,*,#3681,.F.);
#4674=ORIENTED_EDGE('',*,*,#3682,.T.);
#4675=ORIENTED_EDGE('',*,*,#3678,.T.);
#4676=ORIENTED_EDGE('',*,*,#3682,.F.);
#4677=ORIENTED_EDGE('',*,*,#3681,.T.);
#4678=ORIENTED_EDGE('',*,*,#3676,.T.);
#4679=ORIENTED_EDGE('',*,*,#3683,.F.);
#4680=ORIENTED_EDGE('',*,*,#3684,.T.);
#4681=ORIENTED_EDGE('',*,*,#3685,.T.);
#4682=ORIENTED_EDGE('',*,*,#3684,.F.);
#4683=ORIENTED_EDGE('',*,*,#3686,.F.);
#4684=ORIENTED_EDGE('',*,*,#3687,.T.);
#4685=ORIENTED_EDGE('',*,*,#3688,.T.);
#4686=ORIENTED_EDGE('',*,*,#3687,.F.);
#4687=ORIENTED_EDGE('',*,*,#3686,.T.);
#4688=ORIENTED_EDGE('',*,*,#3683,.T.);
#4689=ORIENTED_EDGE('',*,*,#3688,.F.);
#4690=ORIENTED_EDGE('',*,*,#3685,.F.);
#4691=ORIENTED_EDGE('',*,*,#3689,.F.);
#4692=ORIENTED_EDGE('',*,*,#3690,.T.);
#4693=ORIENTED_EDGE('',*,*,#3691,.T.);
#4694=ORIENTED_EDGE('',*,*,#3690,.F.);
#4695=ORIENTED_EDGE('',*,*,#3692,.F.);
#4696=ORIENTED_EDGE('',*,*,#3693,.T.);
#4697=ORIENTED_EDGE('',*,*,#3694,.T.);
#4698=ORIENTED_EDGE('',*,*,#3693,.F.);
#4699=ORIENTED_EDGE('',*,*,#3692,.T.);
#4700=ORIENTED_EDGE('',*,*,#3689,.T.);
#4701=ORIENTED_EDGE('',*,*,#3694,.F.);
#4702=ORIENTED_EDGE('',*,*,#3691,.F.);
#4703=ORIENTED_EDGE('',*,*,#3695,.F.);
#4704=ORIENTED_EDGE('',*,*,#3696,.T.);
#4705=ORIENTED_EDGE('',*,*,#3697,.F.);
#4706=ORIENTED_EDGE('',*,*,#3698,.F.);
#4707=ORIENTED_EDGE('',*,*,#3699,.F.);
#4708=ORIENTED_EDGE('',*,*,#3698,.T.);
#4709=ORIENTED_EDGE('',*,*,#3700,.F.);
#4710=ORIENTED_EDGE('',*,*,#3701,.F.);
#4711=ORIENTED_EDGE('',*,*,#3702,.F.);
#4712=ORIENTED_EDGE('',*,*,#3701,.T.);
#4713=ORIENTED_EDGE('',*,*,#3703,.F.);
#4714=ORIENTED_EDGE('',*,*,#3704,.F.);
#4715=ORIENTED_EDGE('',*,*,#3705,.F.);
#4716=ORIENTED_EDGE('',*,*,#3704,.T.);
#4717=ORIENTED_EDGE('',*,*,#3706,.F.);
#4718=ORIENTED_EDGE('',*,*,#3696,.F.);
#4719=ORIENTED_EDGE('',*,*,#3706,.T.);
#4720=ORIENTED_EDGE('',*,*,#3703,.T.);
#4721=ORIENTED_EDGE('',*,*,#3700,.T.);
#4722=ORIENTED_EDGE('',*,*,#3697,.T.);
#4723=ORIENTED_EDGE('',*,*,#3705,.T.);
#4724=ORIENTED_EDGE('',*,*,#3695,.T.);
#4725=ORIENTED_EDGE('',*,*,#3699,.T.);
#4726=ORIENTED_EDGE('',*,*,#3702,.T.);
#4727=ORIENTED_EDGE('',*,*,#3707,.F.);
#4728=ORIENTED_EDGE('',*,*,#3708,.T.);
#4729=ORIENTED_EDGE('',*,*,#3709,.F.);
#4730=ORIENTED_EDGE('',*,*,#3708,.F.);
#4731=ORIENTED_EDGE('',*,*,#3710,.T.);
#4732=ORIENTED_EDGE('',*,*,#3711,.T.);
#4733=ORIENTED_EDGE('',*,*,#3712,.F.);
#4734=ORIENTED_EDGE('',*,*,#3713,.F.);
#4735=ORIENTED_EDGE('',*,*,#3714,.T.);
#4736=ORIENTED_EDGE('',*,*,#3713,.T.);
#4737=ORIENTED_EDGE('',*,*,#3715,.F.);
#4738=ORIENTED_EDGE('',*,*,#3716,.F.);
#4739=ORIENTED_EDGE('',*,*,#3717,.T.);
#4740=ORIENTED_EDGE('',*,*,#3716,.T.);
#4741=ORIENTED_EDGE('',*,*,#3718,.F.);
#4742=ORIENTED_EDGE('',*,*,#3719,.F.);
#4743=ORIENTED_EDGE('',*,*,#3720,.T.);
#4744=ORIENTED_EDGE('',*,*,#3719,.T.);
#4745=ORIENTED_EDGE('',*,*,#3721,.F.);
#4746=ORIENTED_EDGE('',*,*,#3711,.F.);
#4747=ORIENTED_EDGE('',*,*,#3721,.T.);
#4748=ORIENTED_EDGE('',*,*,#3718,.T.);
#4749=ORIENTED_EDGE('',*,*,#3715,.T.);
#4750=ORIENTED_EDGE('',*,*,#3712,.T.);
#4751=ORIENTED_EDGE('',*,*,#3709,.T.);
#4752=ORIENTED_EDGE('',*,*,#3720,.F.);
#4753=ORIENTED_EDGE('',*,*,#3710,.F.);
#4754=ORIENTED_EDGE('',*,*,#3714,.F.);
#4755=ORIENTED_EDGE('',*,*,#3717,.F.);
#4756=ORIENTED_EDGE('',*,*,#3707,.T.);
#4757=ORIENTED_EDGE('',*,*,#3722,.F.);
#4758=ORIENTED_EDGE('',*,*,#3723,.T.);
#4759=ORIENTED_EDGE('',*,*,#3724,.F.);
#4760=ORIENTED_EDGE('',*,*,#3723,.F.);
#4761=ORIENTED_EDGE('',*,*,#3725,.F.);
#4762=ORIENTED_EDGE('',*,*,#3726,.T.);
#4763=ORIENTED_EDGE('',*,*,#3727,.F.);
#4764=ORIENTED_EDGE('',*,*,#3726,.F.);
#4765=ORIENTED_EDGE('',*,*,#3728,.T.);
#4766=ORIENTED_EDGE('',*,*,#3728,.F.);
#4767=ORIENTED_EDGE('',*,*,#3725,.T.);
#4768=ORIENTED_EDGE('',*,*,#3724,.T.);
#4769=ORIENTED_EDGE('',*,*,#3729,.F.);
#4770=ORIENTED_EDGE('',*,*,#3730,.T.);
#4771=ORIENTED_EDGE('',*,*,#3731,.F.);
#4772=ORIENTED_EDGE('',*,*,#3732,.F.);
#4773=ORIENTED_EDGE('',*,*,#3733,.F.);
#4774=ORIENTED_EDGE('',*,*,#3734,.T.);
#4775=ORIENTED_EDGE('',*,*,#3735,.F.);
#4776=ORIENTED_EDGE('',*,*,#3736,.F.);
#4777=ORIENTED_EDGE('',*,*,#3737,.T.);
#4778=ORIENTED_EDGE('',*,*,#3738,.F.);
#4779=ORIENTED_EDGE('',*,*,#3737,.F.);
#4780=ORIENTED_EDGE('',*,*,#3739,.F.);
#4781=ORIENTED_EDGE('',*,*,#3730,.F.);
#4782=ORIENTED_EDGE('',*,*,#3740,.F.);
#4783=ORIENTED_EDGE('',*,*,#3741,.T.);
#4784=ORIENTED_EDGE('',*,*,#3742,.F.);
#4785=ORIENTED_EDGE('',*,*,#3743,.F.);
#4786=ORIENTED_EDGE('',*,*,#3734,.F.);
#4787=ORIENTED_EDGE('',*,*,#3744,.F.);
#4788=ORIENTED_EDGE('',*,*,#3741,.F.);
#4789=ORIENTED_EDGE('',*,*,#3745,.T.);
#4790=ORIENTED_EDGE('',*,*,#3746,.T.);
#4791=ORIENTED_EDGE('',*,*,#3747,.T.);
#4792=ORIENTED_EDGE('',*,*,#3748,.T.);
#4793=ORIENTED_EDGE('',*,*,#3749,.T.);
#4794=ORIENTED_EDGE('',*,*,#3750,.T.);
#4795=ORIENTED_EDGE('',*,*,#3732,.T.);
#4796=ORIENTED_EDGE('',*,*,#3743,.T.);
#4797=ORIENTED_EDGE('',*,*,#3740,.T.);
#4798=ORIENTED_EDGE('',*,*,#3751,.T.);
#4799=ORIENTED_EDGE('',*,*,#3752,.T.);
#4800=ORIENTED_EDGE('',*,*,#3753,.T.);
#4801=ORIENTED_EDGE('',*,*,#3735,.T.);
#4802=ORIENTED_EDGE('',*,*,#3738,.T.);
#4803=ORIENTED_EDGE('',*,*,#3729,.T.);
#4804=ORIENTED_EDGE('',*,*,#3754,.T.);
#4805=ORIENTED_EDGE('',*,*,#3755,.T.);
#4806=ORIENTED_EDGE('',*,*,#3756,.T.);
#4807=ORIENTED_EDGE('',*,*,#3733,.T.);
#4808=ORIENTED_EDGE('',*,*,#3756,.F.);
#4809=ORIENTED_EDGE('',*,*,#3757,.F.);
#4810=ORIENTED_EDGE('',*,*,#3754,.F.);
#4811=ORIENTED_EDGE('',*,*,#3731,.T.);
#4812=ORIENTED_EDGE('',*,*,#3739,.T.);
#4813=ORIENTED_EDGE('',*,*,#3736,.T.);
#4814=ORIENTED_EDGE('',*,*,#3753,.F.);
#4815=ORIENTED_EDGE('',*,*,#3758,.F.);
#4816=ORIENTED_EDGE('',*,*,#3751,.F.);
#4817=ORIENTED_EDGE('',*,*,#3742,.T.);
#4818=ORIENTED_EDGE('',*,*,#3744,.T.);
#4819=ORIENTED_EDGE('',*,*,#3752,.F.);
#4820=ORIENTED_EDGE('',*,*,#3758,.T.);
#4821=ORIENTED_EDGE('',*,*,#3722,.T.);
#4822=ORIENTED_EDGE('',*,*,#3755,.F.);
#4823=ORIENTED_EDGE('',*,*,#3757,.T.);
#4824=ORIENTED_EDGE('',*,*,#3727,.T.);
#4825=ORIENTED_EDGE('',*,*,#3759,.F.);
#4826=ORIENTED_EDGE('',*,*,#3760,.T.);
#4827=ORIENTED_EDGE('',*,*,#3761,.T.);
#4828=ORIENTED_EDGE('',*,*,#3762,.F.);
#4829=ORIENTED_EDGE('',*,*,#3763,.F.);
#4830=ORIENTED_EDGE('',*,*,#3764,.T.);
#4831=ORIENTED_EDGE('',*,*,#3765,.T.);
#4832=ORIENTED_EDGE('',*,*,#3760,.F.);
#4833=ORIENTED_EDGE('',*,*,#3766,.F.);
#4834=ORIENTED_EDGE('',*,*,#3767,.T.);
#4835=ORIENTED_EDGE('',*,*,#3768,.T.);
#4836=ORIENTED_EDGE('',*,*,#3764,.F.);
#4837=ORIENTED_EDGE('',*,*,#3769,.F.);
#4838=ORIENTED_EDGE('',*,*,#3762,.T.);
#4839=ORIENTED_EDGE('',*,*,#3770,.T.);
#4840=ORIENTED_EDGE('',*,*,#3767,.F.);
#4841=ORIENTED_EDGE('',*,*,#3770,.F.);
#4842=ORIENTED_EDGE('',*,*,#3761,.F.);
#4843=ORIENTED_EDGE('',*,*,#3765,.F.);
#4844=ORIENTED_EDGE('',*,*,#3768,.F.);
#4845=ORIENTED_EDGE('',*,*,#3771,.F.);
#4846=ORIENTED_EDGE('',*,*,#3772,.T.);
#4847=ORIENTED_EDGE('',*,*,#3750,.F.);
#4848=ORIENTED_EDGE('',*,*,#3772,.F.);
#4849=ORIENTED_EDGE('',*,*,#3773,.F.);
#4850=ORIENTED_EDGE('',*,*,#3774,.T.);
#4851=ORIENTED_EDGE('',*,*,#3749,.F.);
#4852=ORIENTED_EDGE('',*,*,#3774,.F.);
#4853=ORIENTED_EDGE('',*,*,#3775,.T.);
#4854=ORIENTED_EDGE('',*,*,#3776,.T.);
#4855=ORIENTED_EDGE('',*,*,#3748,.F.);
#4856=ORIENTED_EDGE('',*,*,#3777,.F.);
#4857=ORIENTED_EDGE('',*,*,#3778,.T.);
#4858=ORIENTED_EDGE('',*,*,#3777,.T.);
#4859=ORIENTED_EDGE('',*,*,#3747,.F.);
#4860=ORIENTED_EDGE('',*,*,#3779,.F.);
#4861=ORIENTED_EDGE('',*,*,#3780,.T.);
#4862=ORIENTED_EDGE('',*,*,#3779,.T.);
#4863=ORIENTED_EDGE('',*,*,#3746,.F.);
#4864=ORIENTED_EDGE('',*,*,#3781,.F.);
#4865=ORIENTED_EDGE('',*,*,#3782,.T.);
#4866=ORIENTED_EDGE('',*,*,#3781,.T.);
#4867=ORIENTED_EDGE('',*,*,#3745,.F.);
#4868=ORIENTED_EDGE('',*,*,#3776,.F.);
#4869=ORIENTED_EDGE('',*,*,#3782,.F.);
#4870=ORIENTED_EDGE('',*,*,#3775,.F.);
#4871=ORIENTED_EDGE('',*,*,#3778,.F.);
#4872=ORIENTED_EDGE('',*,*,#3780,.F.);
#4873=ORIENTED_EDGE('',*,*,#3759,.T.);
#4874=ORIENTED_EDGE('',*,*,#3769,.T.);
#4875=ORIENTED_EDGE('',*,*,#3766,.T.);
#4876=ORIENTED_EDGE('',*,*,#3763,.T.);
#4877=ORIENTED_EDGE('',*,*,#3771,.T.);
#4878=ORIENTED_EDGE('',*,*,#3773,.T.);
#4879=ORIENTED_EDGE('',*,*,#3783,.T.);
#4880=ORIENTED_EDGE('',*,*,#3784,.T.);
#4881=ORIENTED_EDGE('',*,*,#3785,.F.);
#4882=ORIENTED_EDGE('',*,*,#3784,.F.);
#4883=ORIENTED_EDGE('',*,*,#3786,.F.);
#4884=ORIENTED_EDGE('',*,*,#3785,.T.);
#4885=ORIENTED_EDGE('',*,*,#3787,.T.);
#4886=ORIENTED_EDGE('',*,*,#3787,.F.);
#4887=ORIENTED_EDGE('',*,*,#3786,.T.);
#4888=ORIENTED_EDGE('',*,*,#3788,.F.);
#4889=ORIENTED_EDGE('',*,*,#3788,.T.);
#4890=ORIENTED_EDGE('',*,*,#3783,.F.);
#4891=ORIENTED_EDGE('',*,*,#3789,.F.);
#4892=ORIENTED_EDGE('',*,*,#3790,.F.);
#4893=ORIENTED_EDGE('',*,*,#3791,.F.);
#4894=ORIENTED_EDGE('',*,*,#3792,.T.);
#4895=ORIENTED_EDGE('',*,*,#3793,.F.);
#4896=ORIENTED_EDGE('',*,*,#3792,.F.);
#4897=ORIENTED_EDGE('',*,*,#3794,.F.);
#4898=ORIENTED_EDGE('',*,*,#3795,.T.);
#4899=ORIENTED_EDGE('',*,*,#3796,.F.);
#4900=ORIENTED_EDGE('',*,*,#3797,.F.);
#4901=ORIENTED_EDGE('',*,*,#3798,.F.);
#4902=ORIENTED_EDGE('',*,*,#3795,.F.);
#4903=ORIENTED_EDGE('',*,*,#3799,.F.);
#4904=ORIENTED_EDGE('',*,*,#3800,.T.);
#4905=ORIENTED_EDGE('',*,*,#3801,.T.);
#4906=ORIENTED_EDGE('',*,*,#3800,.F.);
#4907=ORIENTED_EDGE('',*,*,#3790,.T.);
#4908=ORIENTED_EDGE('',*,*,#3789,.T.);
#4909=ORIENTED_EDGE('',*,*,#3791,.T.);
#4910=ORIENTED_EDGE('',*,*,#3797,.T.);
#4911=ORIENTED_EDGE('',*,*,#3796,.T.);
#4912=ORIENTED_EDGE('',*,*,#3798,.T.);
#4913=ORIENTED_EDGE('',*,*,#3802,.T.);
#4914=ORIENTED_EDGE('',*,*,#3803,.T.);
#4915=ORIENTED_EDGE('',*,*,#3804,.T.);
#4916=ORIENTED_EDGE('',*,*,#3805,.T.);
#4917=ORIENTED_EDGE('',*,*,#3806,.T.);
#4918=ORIENTED_EDGE('',*,*,#3807,.T.);
#4919=ORIENTED_EDGE('',*,*,#3808,.T.);
#4920=ORIENTED_EDGE('',*,*,#3809,.T.);
#4921=ORIENTED_EDGE('',*,*,#3810,.T.);
#4922=ORIENTED_EDGE('',*,*,#3811,.T.);
#4923=ORIENTED_EDGE('',*,*,#3812,.T.);
#4924=ORIENTED_EDGE('',*,*,#3813,.T.);
#4925=ORIENTED_EDGE('',*,*,#3803,.F.);
#4926=ORIENTED_EDGE('',*,*,#3802,.F.);
#4927=ORIENTED_EDGE('',*,*,#3804,.F.);
#4928=ORIENTED_EDGE('',*,*,#3814,.T.);
#4929=ORIENTED_EDGE('',*,*,#3815,.F.);
#4930=ORIENTED_EDGE('',*,*,#3814,.F.);
#4931=ORIENTED_EDGE('',*,*,#3816,.F.);
#4932=ORIENTED_EDGE('',*,*,#3817,.T.);
#4933=ORIENTED_EDGE('',*,*,#3806,.F.);
#4934=ORIENTED_EDGE('',*,*,#3805,.F.);
#4935=ORIENTED_EDGE('',*,*,#3807,.F.);
#4936=ORIENTED_EDGE('',*,*,#3817,.F.);
#4937=ORIENTED_EDGE('',*,*,#3809,.F.);
#4938=ORIENTED_EDGE('',*,*,#3808,.F.);
#4939=ORIENTED_EDGE('',*,*,#3810,.F.);
#4940=ORIENTED_EDGE('',*,*,#3818,.T.);
#4941=ORIENTED_EDGE('',*,*,#3819,.F.);
#4942=ORIENTED_EDGE('',*,*,#3818,.F.);
#4943=ORIENTED_EDGE('',*,*,#3820,.F.);
#4944=ORIENTED_EDGE('',*,*,#3821,.T.);
#4945=ORIENTED_EDGE('',*,*,#3812,.F.);
#4946=ORIENTED_EDGE('',*,*,#3811,.F.);
#4947=ORIENTED_EDGE('',*,*,#3813,.F.);
#4948=ORIENTED_EDGE('',*,*,#3821,.F.);
#4949=ORIENTED_EDGE('',*,*,#3801,.F.);
#4950=ORIENTED_EDGE('',*,*,#3822,.T.);
#4951=ORIENTED_EDGE('',*,*,#3823,.F.);
#4952=ORIENTED_EDGE('',*,*,#3799,.T.);
#4953=ORIENTED_EDGE('',*,*,#3824,.F.);
#4954=ORIENTED_EDGE('',*,*,#3825,.T.);
#4955=ORIENTED_EDGE('',*,*,#3823,.T.);
#4956=ORIENTED_EDGE('',*,*,#3825,.F.);
#4957=ORIENTED_EDGE('',*,*,#3824,.T.);
#4958=ORIENTED_EDGE('',*,*,#3826,.F.);
#4959=ORIENTED_EDGE('',*,*,#3826,.T.);
#4960=ORIENTED_EDGE('',*,*,#3827,.T.);
#4961=ORIENTED_EDGE('',*,*,#3822,.F.);
#4962=ORIENTED_EDGE('',*,*,#3827,.F.);
#4963=ORIENTED_EDGE('',*,*,#3794,.T.);
#4964=ORIENTED_EDGE('',*,*,#3793,.T.);
#4965=ORIENTED_EDGE('',*,*,#3816,.T.);
#4966=ORIENTED_EDGE('',*,*,#3815,.T.);
#4967=ORIENTED_EDGE('',*,*,#3820,.T.);
#4968=ORIENTED_EDGE('',*,*,#3819,.T.);
#4969=ORIENTED_EDGE('',*,*,#3828,.F.);
#4970=ORIENTED_EDGE('',*,*,#3829,.T.);
#4971=ORIENTED_EDGE('',*,*,#3830,.T.);
#4972=ORIENTED_EDGE('',*,*,#3829,.F.);
#4973=ORIENTED_EDGE('',*,*,#3831,.F.);
#4974=ORIENTED_EDGE('',*,*,#3832,.T.);
#4975=ORIENTED_EDGE('',*,*,#3833,.T.);
#4976=ORIENTED_EDGE('',*,*,#3832,.F.);
#4977=ORIENTED_EDGE('',*,*,#3831,.T.);
#4978=ORIENTED_EDGE('',*,*,#3828,.T.);
#4979=ORIENTED_EDGE('',*,*,#3833,.F.);
#4980=ORIENTED_EDGE('',*,*,#3830,.F.);
#4981=ORIENTED_EDGE('',*,*,#3834,.T.);
#4982=ORIENTED_EDGE('',*,*,#3835,.T.);
#4983=ORIENTED_EDGE('',*,*,#3836,.T.);
#4984=ORIENTED_EDGE('',*,*,#3837,.F.);
#4985=ORIENTED_EDGE('',*,*,#3838,.T.);
#4986=ORIENTED_EDGE('',*,*,#3839,.T.);
#4987=ORIENTED_EDGE('',*,*,#3840,.T.);
#4988=ORIENTED_EDGE('',*,*,#3835,.F.);
#4989=ORIENTED_EDGE('',*,*,#3841,.T.);
#4990=ORIENTED_EDGE('',*,*,#3842,.T.);
#4991=ORIENTED_EDGE('',*,*,#3843,.T.);
#4992=ORIENTED_EDGE('',*,*,#3839,.F.);
#4993=ORIENTED_EDGE('',*,*,#3844,.T.);
#4994=ORIENTED_EDGE('',*,*,#3845,.T.);
#4995=ORIENTED_EDGE('',*,*,#3846,.T.);
#4996=ORIENTED_EDGE('',*,*,#3842,.F.);
#4997=ORIENTED_EDGE('',*,*,#3847,.T.);
#4998=ORIENTED_EDGE('',*,*,#3848,.T.);
#4999=ORIENTED_EDGE('',*,*,#3849,.T.);
#5000=ORIENTED_EDGE('',*,*,#3845,.F.);
#5001=ORIENTED_EDGE('',*,*,#3850,.T.);
#5002=ORIENTED_EDGE('',*,*,#3837,.T.);
#5003=ORIENTED_EDGE('',*,*,#3851,.T.);
#5004=ORIENTED_EDGE('',*,*,#3848,.F.);
#5005=ORIENTED_EDGE('',*,*,#3850,.F.);
#5006=ORIENTED_EDGE('',*,*,#3847,.F.);
#5007=ORIENTED_EDGE('',*,*,#3844,.F.);
#5008=ORIENTED_EDGE('',*,*,#3841,.F.);
#5009=ORIENTED_EDGE('',*,*,#3838,.F.);
#5010=ORIENTED_EDGE('',*,*,#3834,.F.);
#5011=ORIENTED_EDGE('',*,*,#3851,.F.);
#5012=ORIENTED_EDGE('',*,*,#3836,.F.);
#5013=ORIENTED_EDGE('',*,*,#3840,.F.);
#5014=ORIENTED_EDGE('',*,*,#3843,.F.);
#5015=ORIENTED_EDGE('',*,*,#3846,.F.);
#5016=ORIENTED_EDGE('',*,*,#3849,.F.);
#5017=ORIENTED_EDGE('',*,*,#3852,.F.);
#5018=ORIENTED_EDGE('',*,*,#3853,.F.);
#5019=ORIENTED_EDGE('',*,*,#3854,.F.);
#5020=ORIENTED_EDGE('',*,*,#3855,.T.);
#5021=ORIENTED_EDGE('',*,*,#3853,.T.);
#5022=ORIENTED_EDGE('',*,*,#3855,.F.);
#5023=ORIENTED_EDGE('',*,*,#3856,.F.);
#5024=ORIENTED_EDGE('',*,*,#3857,.T.);
#5025=ORIENTED_EDGE('',*,*,#3854,.T.);
#5026=ORIENTED_EDGE('',*,*,#3857,.F.);
#5027=ORIENTED_EDGE('',*,*,#3858,.F.);
#5028=ORIENTED_EDGE('',*,*,#3859,.T.);
#5029=ORIENTED_EDGE('',*,*,#3856,.T.);
#5030=ORIENTED_EDGE('',*,*,#3859,.F.);
#5031=ORIENTED_EDGE('',*,*,#3858,.T.);
#5032=ORIENTED_EDGE('',*,*,#3860,.F.);
#5033=ORIENTED_EDGE('',*,*,#3861,.F.);
#5034=ORIENTED_EDGE('',*,*,#3862,.T.);
#5035=ORIENTED_EDGE('',*,*,#3860,.T.);
#5036=ORIENTED_EDGE('',*,*,#3862,.F.);
#5037=ORIENTED_EDGE('',*,*,#3852,.T.);
#5038=ORIENTED_EDGE('',*,*,#3863,.T.);
#5039=ORIENTED_EDGE('',*,*,#3861,.T.);
#5040=ORIENTED_EDGE('',*,*,#3863,.F.);
#5041=ORIENTED_EDGE('',*,*,#3864,.T.);
#5042=ORIENTED_EDGE('',*,*,#3865,.T.);
#5043=ORIENTED_EDGE('',*,*,#3866,.T.);
#5044=ORIENTED_EDGE('',*,*,#3867,.F.);
#5045=ORIENTED_EDGE('',*,*,#3868,.T.);
#5046=ORIENTED_EDGE('',*,*,#3869,.T.);
#5047=ORIENTED_EDGE('',*,*,#3870,.T.);
#5048=ORIENTED_EDGE('',*,*,#3865,.F.);
#5049=ORIENTED_EDGE('',*,*,#3871,.T.);
#5050=ORIENTED_EDGE('',*,*,#3872,.T.);
#5051=ORIENTED_EDGE('',*,*,#3873,.T.);
#5052=ORIENTED_EDGE('',*,*,#3869,.F.);
#5053=ORIENTED_EDGE('',*,*,#3874,.T.);
#5054=ORIENTED_EDGE('',*,*,#3875,.T.);
#5055=ORIENTED_EDGE('',*,*,#3876,.T.);
#5056=ORIENTED_EDGE('',*,*,#3872,.F.);
#5057=ORIENTED_EDGE('',*,*,#3877,.T.);
#5058=ORIENTED_EDGE('',*,*,#3878,.T.);
#5059=ORIENTED_EDGE('',*,*,#3879,.T.);
#5060=ORIENTED_EDGE('',*,*,#3875,.F.);
#5061=ORIENTED_EDGE('',*,*,#3880,.T.);
#5062=ORIENTED_EDGE('',*,*,#3867,.T.);
#5063=ORIENTED_EDGE('',*,*,#3881,.T.);
#5064=ORIENTED_EDGE('',*,*,#3878,.F.);
#5065=ORIENTED_EDGE('',*,*,#3880,.F.);
#5066=ORIENTED_EDGE('',*,*,#3877,.F.);
#5067=ORIENTED_EDGE('',*,*,#3874,.F.);
#5068=ORIENTED_EDGE('',*,*,#3871,.F.);
#5069=ORIENTED_EDGE('',*,*,#3868,.F.);
#5070=ORIENTED_EDGE('',*,*,#3864,.F.);
#5071=ORIENTED_EDGE('',*,*,#3881,.F.);
#5072=ORIENTED_EDGE('',*,*,#3866,.F.);
#5073=ORIENTED_EDGE('',*,*,#3870,.F.);
#5074=ORIENTED_EDGE('',*,*,#3873,.F.);
#5075=ORIENTED_EDGE('',*,*,#3876,.F.);
#5076=ORIENTED_EDGE('',*,*,#3879,.F.);
#5077=ORIENTED_EDGE('',*,*,#3882,.F.);
#5078=ORIENTED_EDGE('',*,*,#3883,.F.);
#5079=ORIENTED_EDGE('',*,*,#3884,.F.);
#5080=ORIENTED_EDGE('',*,*,#3885,.T.);
#5081=ORIENTED_EDGE('',*,*,#3883,.T.);
#5082=ORIENTED_EDGE('',*,*,#3885,.F.);
#5083=ORIENTED_EDGE('',*,*,#3886,.F.);
#5084=ORIENTED_EDGE('',*,*,#3887,.T.);
#5085=ORIENTED_EDGE('',*,*,#3884,.T.);
#5086=ORIENTED_EDGE('',*,*,#3887,.F.);
#5087=ORIENTED_EDGE('',*,*,#3888,.F.);
#5088=ORIENTED_EDGE('',*,*,#3889,.T.);
#5089=ORIENTED_EDGE('',*,*,#3886,.T.);
#5090=ORIENTED_EDGE('',*,*,#3889,.F.);
#5091=ORIENTED_EDGE('',*,*,#3888,.T.);
#5092=ORIENTED_EDGE('',*,*,#3890,.F.);
#5093=ORIENTED_EDGE('',*,*,#3891,.F.);
#5094=ORIENTED_EDGE('',*,*,#3892,.T.);
#5095=ORIENTED_EDGE('',*,*,#3890,.T.);
#5096=ORIENTED_EDGE('',*,*,#3892,.F.);
#5097=ORIENTED_EDGE('',*,*,#3882,.T.);
#5098=ORIENTED_EDGE('',*,*,#3893,.T.);
#5099=ORIENTED_EDGE('',*,*,#3891,.T.);
#5100=ORIENTED_EDGE('',*,*,#3893,.F.);
#5101=ORIENTED_EDGE('',*,*,#3894,.F.);
#5102=ORIENTED_EDGE('',*,*,#3895,.T.);
#5103=ORIENTED_EDGE('',*,*,#3896,.T.);
#5104=ORIENTED_EDGE('',*,*,#3895,.F.);
#5105=ORIENTED_EDGE('',*,*,#3894,.T.);
#5106=ORIENTED_EDGE('',*,*,#3896,.F.);
#5107=ORIENTED_EDGE('',*,*,#3897,.F.);
#5108=ORIENTED_EDGE('',*,*,#3898,.T.);
#5109=ORIENTED_EDGE('',*,*,#3899,.F.);
#5110=ORIENTED_EDGE('',*,*,#3900,.F.);
#5111=ORIENTED_EDGE('',*,*,#3901,.T.);
#5112=ORIENTED_EDGE('',*,*,#3902,.F.);
#5113=ORIENTED_EDGE('',*,*,#3903,.F.);
#5114=ORIENTED_EDGE('',*,*,#3901,.F.);
#5115=ORIENTED_EDGE('',*,*,#3904,.F.);
#5116=ORIENTED_EDGE('',*,*,#3905,.F.);
#5117=ORIENTED_EDGE('',*,*,#3898,.F.);
#5118=ORIENTED_EDGE('',*,*,#3906,.F.);
#5119=ORIENTED_EDGE('',*,*,#3904,.T.);
#5120=ORIENTED_EDGE('',*,*,#3900,.T.);
#5121=ORIENTED_EDGE('',*,*,#3907,.F.);
#5122=ORIENTED_EDGE('',*,*,#3908,.T.);
#5123=ORIENTED_EDGE('',*,*,#3909,.T.);
#5124=ORIENTED_EDGE('',*,*,#3908,.F.);
#5125=ORIENTED_EDGE('',*,*,#3905,.T.);
#5126=ORIENTED_EDGE('',*,*,#3906,.T.);
#5127=ORIENTED_EDGE('',*,*,#3899,.T.);
#5128=ORIENTED_EDGE('',*,*,#3897,.T.);
#5129=ORIENTED_EDGE('',*,*,#3910,.F.);
#5130=ORIENTED_EDGE('',*,*,#3911,.T.);
#5131=ORIENTED_EDGE('',*,*,#3912,.T.);
#5132=ORIENTED_EDGE('',*,*,#3911,.F.);
#5133=ORIENTED_EDGE('',*,*,#3902,.T.);
#5134=ORIENTED_EDGE('',*,*,#3903,.T.);
#5135=ORIENTED_EDGE('',*,*,#3910,.T.);
#5136=ORIENTED_EDGE('',*,*,#3907,.T.);
#5137=ORIENTED_EDGE('',*,*,#3912,.F.);
#5138=ORIENTED_EDGE('',*,*,#3909,.F.);
#5139=ORIENTED_EDGE('',*,*,#3913,.F.);
#5140=ORIENTED_EDGE('',*,*,#3914,.T.);
#5141=ORIENTED_EDGE('',*,*,#3915,.F.);
#5142=ORIENTED_EDGE('',*,*,#3916,.F.);
#5143=ORIENTED_EDGE('',*,*,#3917,.T.);
#5144=ORIENTED_EDGE('',*,*,#3918,.F.);
#5145=ORIENTED_EDGE('',*,*,#3919,.F.);
#5146=ORIENTED_EDGE('',*,*,#3917,.F.);
#5147=ORIENTED_EDGE('',*,*,#3920,.F.);
#5148=ORIENTED_EDGE('',*,*,#3921,.F.);
#5149=ORIENTED_EDGE('',*,*,#3914,.F.);
#5150=ORIENTED_EDGE('',*,*,#3922,.F.);
#5151=ORIENTED_EDGE('',*,*,#3920,.T.);
#5152=ORIENTED_EDGE('',*,*,#3916,.T.);
#5153=ORIENTED_EDGE('',*,*,#3923,.F.);
#5154=ORIENTED_EDGE('',*,*,#3924,.T.);
#5155=ORIENTED_EDGE('',*,*,#3925,.T.);
#5156=ORIENTED_EDGE('',*,*,#3924,.F.);
#5157=ORIENTED_EDGE('',*,*,#3921,.T.);
#5158=ORIENTED_EDGE('',*,*,#3922,.T.);
#5159=ORIENTED_EDGE('',*,*,#3915,.T.);
#5160=ORIENTED_EDGE('',*,*,#3913,.T.);
#5161=ORIENTED_EDGE('',*,*,#3926,.F.);
#5162=ORIENTED_EDGE('',*,*,#3927,.T.);
#5163=ORIENTED_EDGE('',*,*,#3928,.T.);
#5164=ORIENTED_EDGE('',*,*,#3927,.F.);
#5165=ORIENTED_EDGE('',*,*,#3918,.T.);
#5166=ORIENTED_EDGE('',*,*,#3919,.T.);
#5167=ORIENTED_EDGE('',*,*,#3926,.T.);
#5168=ORIENTED_EDGE('',*,*,#3923,.T.);
#5169=ORIENTED_EDGE('',*,*,#3928,.F.);
#5170=ORIENTED_EDGE('',*,*,#3925,.F.);
#5171=ORIENTED_EDGE('',*,*,#3929,.F.);
#5172=ORIENTED_EDGE('',*,*,#3930,.T.);
#5173=ORIENTED_EDGE('',*,*,#3931,.T.);
#5174=ORIENTED_EDGE('',*,*,#3930,.F.);
#5175=ORIENTED_EDGE('',*,*,#3932,.F.);
#5176=ORIENTED_EDGE('',*,*,#3933,.T.);
#5177=ORIENTED_EDGE('',*,*,#3934,.T.);
#5178=ORIENTED_EDGE('',*,*,#3933,.F.);
#5179=ORIENTED_EDGE('',*,*,#3932,.T.);
#5180=ORIENTED_EDGE('',*,*,#3929,.T.);
#5181=ORIENTED_EDGE('',*,*,#3934,.F.);
#5182=ORIENTED_EDGE('',*,*,#3931,.F.);
#5183=ORIENTED_EDGE('',*,*,#3935,.F.);
#5184=ORIENTED_EDGE('',*,*,#3936,.T.);
#5185=ORIENTED_EDGE('',*,*,#3937,.T.);
#5186=ORIENTED_EDGE('',*,*,#3936,.F.);
#5187=ORIENTED_EDGE('',*,*,#3938,.F.);
#5188=ORIENTED_EDGE('',*,*,#3939,.T.);
#5189=ORIENTED_EDGE('',*,*,#3940,.T.);
#5190=ORIENTED_EDGE('',*,*,#3939,.F.);
#5191=ORIENTED_EDGE('',*,*,#3938,.T.);
#5192=ORIENTED_EDGE('',*,*,#3935,.T.);
#5193=ORIENTED_EDGE('',*,*,#3940,.F.);
#5194=ORIENTED_EDGE('',*,*,#3937,.F.);
#5195=ORIENTED_EDGE('',*,*,#3941,.F.);
#5196=ORIENTED_EDGE('',*,*,#3942,.T.);
#5197=ORIENTED_EDGE('',*,*,#3943,.F.);
#5198=ORIENTED_EDGE('',*,*,#3944,.F.);
#5199=ORIENTED_EDGE('',*,*,#3945,.T.);
#5200=ORIENTED_EDGE('',*,*,#3946,.F.);
#5201=ORIENTED_EDGE('',*,*,#3947,.F.);
#5202=ORIENTED_EDGE('',*,*,#3945,.F.);
#5203=ORIENTED_EDGE('',*,*,#3948,.F.);
#5204=ORIENTED_EDGE('',*,*,#3949,.F.);
#5205=ORIENTED_EDGE('',*,*,#3942,.F.);
#5206=ORIENTED_EDGE('',*,*,#3950,.F.);
#5207=ORIENTED_EDGE('',*,*,#3948,.T.);
#5208=ORIENTED_EDGE('',*,*,#3944,.T.);
#5209=ORIENTED_EDGE('',*,*,#3951,.F.);
#5210=ORIENTED_EDGE('',*,*,#3952,.T.);
#5211=ORIENTED_EDGE('',*,*,#3953,.T.);
#5212=ORIENTED_EDGE('',*,*,#3952,.F.);
#5213=ORIENTED_EDGE('',*,*,#3949,.T.);
#5214=ORIENTED_EDGE('',*,*,#3950,.T.);
#5215=ORIENTED_EDGE('',*,*,#3943,.T.);
#5216=ORIENTED_EDGE('',*,*,#3941,.T.);
#5217=ORIENTED_EDGE('',*,*,#3954,.F.);
#5218=ORIENTED_EDGE('',*,*,#3955,.T.);
#5219=ORIENTED_EDGE('',*,*,#3956,.T.);
#5220=ORIENTED_EDGE('',*,*,#3955,.F.);
#5221=ORIENTED_EDGE('',*,*,#3946,.T.);
#5222=ORIENTED_EDGE('',*,*,#3947,.T.);
#5223=ORIENTED_EDGE('',*,*,#3954,.T.);
#5224=ORIENTED_EDGE('',*,*,#3951,.T.);
#5225=ORIENTED_EDGE('',*,*,#3956,.F.);
#5226=ORIENTED_EDGE('',*,*,#3953,.F.);
#5227=ORIENTED_EDGE('',*,*,#3957,.F.);
#5228=ORIENTED_EDGE('',*,*,#3958,.T.);
#5229=ORIENTED_EDGE('',*,*,#3959,.T.);
#5230=ORIENTED_EDGE('',*,*,#3958,.F.);
#5231=ORIENTED_EDGE('',*,*,#3960,.F.);
#5232=ORIENTED_EDGE('',*,*,#3961,.T.);
#5233=ORIENTED_EDGE('',*,*,#3962,.T.);
#5234=ORIENTED_EDGE('',*,*,#3961,.F.);
#5235=ORIENTED_EDGE('',*,*,#3960,.T.);
#5236=ORIENTED_EDGE('',*,*,#3957,.T.);
#5237=ORIENTED_EDGE('',*,*,#3962,.F.);
#5238=ORIENTED_EDGE('',*,*,#3959,.F.);
#5239=ORIENTED_EDGE('',*,*,#3963,.F.);
#5240=ORIENTED_EDGE('',*,*,#3964,.T.);
#5241=ORIENTED_EDGE('',*,*,#3965,.F.);
#5242=ORIENTED_EDGE('',*,*,#3966,.F.);
#5243=ORIENTED_EDGE('',*,*,#3967,.T.);
#5244=ORIENTED_EDGE('',*,*,#3968,.F.);
#5245=ORIENTED_EDGE('',*,*,#3969,.F.);
#5246=ORIENTED_EDGE('',*,*,#3967,.F.);
#5247=ORIENTED_EDGE('',*,*,#3970,.F.);
#5248=ORIENTED_EDGE('',*,*,#3971,.F.);
#5249=ORIENTED_EDGE('',*,*,#3964,.F.);
#5250=ORIENTED_EDGE('',*,*,#3972,.F.);
#5251=ORIENTED_EDGE('',*,*,#3970,.T.);
#5252=ORIENTED_EDGE('',*,*,#3966,.T.);
#5253=ORIENTED_EDGE('',*,*,#3973,.F.);
#5254=ORIENTED_EDGE('',*,*,#3974,.T.);
#5255=ORIENTED_EDGE('',*,*,#3975,.T.);
#5256=ORIENTED_EDGE('',*,*,#3974,.F.);
#5257=ORIENTED_EDGE('',*,*,#3971,.T.);
#5258=ORIENTED_EDGE('',*,*,#3972,.T.);
#5259=ORIENTED_EDGE('',*,*,#3965,.T.);
#5260=ORIENTED_EDGE('',*,*,#3963,.T.);
#5261=ORIENTED_EDGE('',*,*,#3976,.F.);
#5262=ORIENTED_EDGE('',*,*,#3977,.T.);
#5263=ORIENTED_EDGE('',*,*,#3978,.T.);
#5264=ORIENTED_EDGE('',*,*,#3977,.F.);
#5265=ORIENTED_EDGE('',*,*,#3968,.T.);
#5266=ORIENTED_EDGE('',*,*,#3969,.T.);
#5267=ORIENTED_EDGE('',*,*,#3976,.T.);
#5268=ORIENTED_EDGE('',*,*,#3973,.T.);
#5269=ORIENTED_EDGE('',*,*,#3978,.F.);
#5270=ORIENTED_EDGE('',*,*,#3975,.F.);
#5271=ORIENTED_EDGE('',*,*,#3979,.F.);
#5272=ORIENTED_EDGE('',*,*,#3980,.T.);
#5273=ORIENTED_EDGE('',*,*,#3981,.F.);
#5274=ORIENTED_EDGE('',*,*,#3982,.F.);
#5275=ORIENTED_EDGE('',*,*,#3983,.T.);
#5276=ORIENTED_EDGE('',*,*,#3984,.F.);
#5277=ORIENTED_EDGE('',*,*,#3985,.F.);
#5278=ORIENTED_EDGE('',*,*,#3983,.F.);
#5279=ORIENTED_EDGE('',*,*,#3986,.F.);
#5280=ORIENTED_EDGE('',*,*,#3987,.F.);
#5281=ORIENTED_EDGE('',*,*,#3980,.F.);
#5282=ORIENTED_EDGE('',*,*,#3988,.F.);
#5283=ORIENTED_EDGE('',*,*,#3986,.T.);
#5284=ORIENTED_EDGE('',*,*,#3982,.T.);
#5285=ORIENTED_EDGE('',*,*,#3989,.F.);
#5286=ORIENTED_EDGE('',*,*,#3990,.T.);
#5287=ORIENTED_EDGE('',*,*,#3991,.F.);
#5288=ORIENTED_EDGE('',*,*,#3990,.F.);
#5289=ORIENTED_EDGE('',*,*,#3984,.T.);
#5290=ORIENTED_EDGE('',*,*,#3985,.T.);
#5291=ORIENTED_EDGE('',*,*,#3989,.T.);
#5292=ORIENTED_EDGE('',*,*,#3992,.T.);
#5293=ORIENTED_EDGE('',*,*,#3993,.F.);
#5294=ORIENTED_EDGE('',*,*,#3994,.T.);
#5295=ORIENTED_EDGE('',*,*,#3992,.F.);
#5296=ORIENTED_EDGE('',*,*,#3994,.F.);
#5297=ORIENTED_EDGE('',*,*,#3987,.T.);
#5298=ORIENTED_EDGE('',*,*,#3988,.T.);
#5299=ORIENTED_EDGE('',*,*,#3981,.T.);
#5300=ORIENTED_EDGE('',*,*,#3979,.T.);
#5301=ORIENTED_EDGE('',*,*,#3995,.F.);
#5302=ORIENTED_EDGE('',*,*,#3996,.T.);
#5303=ORIENTED_EDGE('',*,*,#3997,.F.);
#5304=ORIENTED_EDGE('',*,*,#3998,.F.);
#5305=ORIENTED_EDGE('',*,*,#3999,.F.);
#5306=ORIENTED_EDGE('',*,*,#3998,.T.);
#5307=ORIENTED_EDGE('',*,*,#4000,.F.);
#5308=ORIENTED_EDGE('',*,*,#4001,.F.);
#5309=ORIENTED_EDGE('',*,*,#4002,.F.);
#5310=ORIENTED_EDGE('',*,*,#4001,.T.);
#5311=ORIENTED_EDGE('',*,*,#4003,.F.);
#5312=ORIENTED_EDGE('',*,*,#4004,.F.);
#5313=ORIENTED_EDGE('',*,*,#4005,.F.);
#5314=ORIENTED_EDGE('',*,*,#4004,.T.);
#5315=ORIENTED_EDGE('',*,*,#4006,.F.);
#5316=ORIENTED_EDGE('',*,*,#4007,.F.);
#5317=ORIENTED_EDGE('',*,*,#4008,.F.);
#5318=ORIENTED_EDGE('',*,*,#4007,.T.);
#5319=ORIENTED_EDGE('',*,*,#4009,.F.);
#5320=ORIENTED_EDGE('',*,*,#4010,.F.);
#5321=ORIENTED_EDGE('',*,*,#4011,.F.);
#5322=ORIENTED_EDGE('',*,*,#4010,.T.);
#5323=ORIENTED_EDGE('',*,*,#4012,.F.);
#5324=ORIENTED_EDGE('',*,*,#4013,.F.);
#5325=ORIENTED_EDGE('',*,*,#4014,.F.);
#5326=ORIENTED_EDGE('',*,*,#4013,.T.);
#5327=ORIENTED_EDGE('',*,*,#4015,.F.);
#5328=ORIENTED_EDGE('',*,*,#4016,.F.);
#5329=ORIENTED_EDGE('',*,*,#4017,.F.);
#5330=ORIENTED_EDGE('',*,*,#4016,.T.);
#5331=ORIENTED_EDGE('',*,*,#4018,.F.);
#5332=ORIENTED_EDGE('',*,*,#4019,.F.);
#5333=ORIENTED_EDGE('',*,*,#4020,.F.);
#5334=ORIENTED_EDGE('',*,*,#4019,.T.);
#5335=ORIENTED_EDGE('',*,*,#4021,.F.);
#5336=ORIENTED_EDGE('',*,*,#4022,.F.);
#5337=ORIENTED_EDGE('',*,*,#4023,.F.);
#5338=ORIENTED_EDGE('',*,*,#4022,.T.);
#5339=ORIENTED_EDGE('',*,*,#4024,.F.);
#5340=ORIENTED_EDGE('',*,*,#4025,.F.);
#5341=ORIENTED_EDGE('',*,*,#4026,.F.);
#5342=ORIENTED_EDGE('',*,*,#4025,.T.);
#5343=ORIENTED_EDGE('',*,*,#4027,.F.);
#5344=ORIENTED_EDGE('',*,*,#4028,.F.);
#5345=ORIENTED_EDGE('',*,*,#4029,.F.);
#5346=ORIENTED_EDGE('',*,*,#4028,.T.);
#5347=ORIENTED_EDGE('',*,*,#4030,.F.);
#5348=ORIENTED_EDGE('',*,*,#4031,.F.);
#5349=ORIENTED_EDGE('',*,*,#4032,.F.);
#5350=ORIENTED_EDGE('',*,*,#4031,.T.);
#5351=ORIENTED_EDGE('',*,*,#4033,.F.);
#5352=ORIENTED_EDGE('',*,*,#4034,.F.);
#5353=ORIENTED_EDGE('',*,*,#4035,.F.);
#5354=ORIENTED_EDGE('',*,*,#4034,.T.);
#5355=ORIENTED_EDGE('',*,*,#4036,.F.);
#5356=ORIENTED_EDGE('',*,*,#4037,.F.);
#5357=ORIENTED_EDGE('',*,*,#4038,.F.);
#5358=ORIENTED_EDGE('',*,*,#4037,.T.);
#5359=ORIENTED_EDGE('',*,*,#4039,.F.);
#5360=ORIENTED_EDGE('',*,*,#4040,.F.);
#5361=ORIENTED_EDGE('',*,*,#4041,.F.);
#5362=ORIENTED_EDGE('',*,*,#4040,.T.);
#5363=ORIENTED_EDGE('',*,*,#4042,.F.);
#5364=ORIENTED_EDGE('',*,*,#4043,.F.);
#5365=ORIENTED_EDGE('',*,*,#4044,.F.);
#5366=ORIENTED_EDGE('',*,*,#4043,.T.);
#5367=ORIENTED_EDGE('',*,*,#4045,.F.);
#5368=ORIENTED_EDGE('',*,*,#4046,.F.);
#5369=ORIENTED_EDGE('',*,*,#4047,.F.);
#5370=ORIENTED_EDGE('',*,*,#4046,.T.);
#5371=ORIENTED_EDGE('',*,*,#4048,.F.);
#5372=ORIENTED_EDGE('',*,*,#4049,.F.);
#5373=ORIENTED_EDGE('',*,*,#4050,.F.);
#5374=ORIENTED_EDGE('',*,*,#4049,.T.);
#5375=ORIENTED_EDGE('',*,*,#4051,.F.);
#5376=ORIENTED_EDGE('',*,*,#4052,.F.);
#5377=ORIENTED_EDGE('',*,*,#4053,.F.);
#5378=ORIENTED_EDGE('',*,*,#4052,.T.);
#5379=ORIENTED_EDGE('',*,*,#4054,.F.);
#5380=ORIENTED_EDGE('',*,*,#4055,.F.);
#5381=ORIENTED_EDGE('',*,*,#4056,.F.);
#5382=ORIENTED_EDGE('',*,*,#4055,.T.);
#5383=ORIENTED_EDGE('',*,*,#4057,.F.);
#5384=ORIENTED_EDGE('',*,*,#4058,.F.);
#5385=ORIENTED_EDGE('',*,*,#4059,.F.);
#5386=ORIENTED_EDGE('',*,*,#4058,.T.);
#5387=ORIENTED_EDGE('',*,*,#4060,.F.);
#5388=ORIENTED_EDGE('',*,*,#4061,.F.);
#5389=ORIENTED_EDGE('',*,*,#4062,.F.);
#5390=ORIENTED_EDGE('',*,*,#4061,.T.);
#5391=ORIENTED_EDGE('',*,*,#4063,.F.);
#5392=ORIENTED_EDGE('',*,*,#4064,.F.);
#5393=ORIENTED_EDGE('',*,*,#4065,.F.);
#5394=ORIENTED_EDGE('',*,*,#4064,.T.);
#5395=ORIENTED_EDGE('',*,*,#4066,.F.);
#5396=ORIENTED_EDGE('',*,*,#4067,.F.);
#5397=ORIENTED_EDGE('',*,*,#4068,.F.);
#5398=ORIENTED_EDGE('',*,*,#4067,.T.);
#5399=ORIENTED_EDGE('',*,*,#4069,.F.);
#5400=ORIENTED_EDGE('',*,*,#4070,.F.);
#5401=ORIENTED_EDGE('',*,*,#4071,.F.);
#5402=ORIENTED_EDGE('',*,*,#4070,.T.);
#5403=ORIENTED_EDGE('',*,*,#4072,.F.);
#5404=ORIENTED_EDGE('',*,*,#4073,.F.);
#5405=ORIENTED_EDGE('',*,*,#4074,.F.);
#5406=ORIENTED_EDGE('',*,*,#4073,.T.);
#5407=ORIENTED_EDGE('',*,*,#4075,.F.);
#5408=ORIENTED_EDGE('',*,*,#4076,.F.);
#5409=ORIENTED_EDGE('',*,*,#4077,.F.);
#5410=ORIENTED_EDGE('',*,*,#4076,.T.);
#5411=ORIENTED_EDGE('',*,*,#4078,.F.);
#5412=ORIENTED_EDGE('',*,*,#4079,.F.);
#5413=ORIENTED_EDGE('',*,*,#4080,.F.);
#5414=ORIENTED_EDGE('',*,*,#4079,.T.);
#5415=ORIENTED_EDGE('',*,*,#4081,.F.);
#5416=ORIENTED_EDGE('',*,*,#4082,.F.);
#5417=ORIENTED_EDGE('',*,*,#4083,.F.);
#5418=ORIENTED_EDGE('',*,*,#4082,.T.);
#5419=ORIENTED_EDGE('',*,*,#4084,.F.);
#5420=ORIENTED_EDGE('',*,*,#4085,.F.);
#5421=ORIENTED_EDGE('',*,*,#4086,.F.);
#5422=ORIENTED_EDGE('',*,*,#4085,.T.);
#5423=ORIENTED_EDGE('',*,*,#4087,.F.);
#5424=ORIENTED_EDGE('',*,*,#4088,.F.);
#5425=ORIENTED_EDGE('',*,*,#4089,.F.);
#5426=ORIENTED_EDGE('',*,*,#4088,.T.);
#5427=ORIENTED_EDGE('',*,*,#4090,.F.);
#5428=ORIENTED_EDGE('',*,*,#4091,.F.);
#5429=ORIENTED_EDGE('',*,*,#4092,.F.);
#5430=ORIENTED_EDGE('',*,*,#4091,.T.);
#5431=ORIENTED_EDGE('',*,*,#4093,.F.);
#5432=ORIENTED_EDGE('',*,*,#4094,.F.);
#5433=ORIENTED_EDGE('',*,*,#4095,.F.);
#5434=ORIENTED_EDGE('',*,*,#4094,.T.);
#5435=ORIENTED_EDGE('',*,*,#4096,.F.);
#5436=ORIENTED_EDGE('',*,*,#4097,.F.);
#5437=ORIENTED_EDGE('',*,*,#4098,.F.);
#5438=ORIENTED_EDGE('',*,*,#4097,.T.);
#5439=ORIENTED_EDGE('',*,*,#4099,.F.);
#5440=ORIENTED_EDGE('',*,*,#4100,.F.);
#5441=ORIENTED_EDGE('',*,*,#4101,.F.);
#5442=ORIENTED_EDGE('',*,*,#4100,.T.);
#5443=ORIENTED_EDGE('',*,*,#4102,.F.);
#5444=ORIENTED_EDGE('',*,*,#4103,.F.);
#5445=ORIENTED_EDGE('',*,*,#4104,.F.);
#5446=ORIENTED_EDGE('',*,*,#4103,.T.);
#5447=ORIENTED_EDGE('',*,*,#4105,.F.);
#5448=ORIENTED_EDGE('',*,*,#4106,.F.);
#5449=ORIENTED_EDGE('',*,*,#4107,.F.);
#5450=ORIENTED_EDGE('',*,*,#4106,.T.);
#5451=ORIENTED_EDGE('',*,*,#4108,.F.);
#5452=ORIENTED_EDGE('',*,*,#4109,.F.);
#5453=ORIENTED_EDGE('',*,*,#4110,.F.);
#5454=ORIENTED_EDGE('',*,*,#4109,.T.);
#5455=ORIENTED_EDGE('',*,*,#4111,.F.);
#5456=ORIENTED_EDGE('',*,*,#4112,.F.);
#5457=ORIENTED_EDGE('',*,*,#4113,.F.);
#5458=ORIENTED_EDGE('',*,*,#4112,.T.);
#5459=ORIENTED_EDGE('',*,*,#4114,.F.);
#5460=ORIENTED_EDGE('',*,*,#4115,.F.);
#5461=ORIENTED_EDGE('',*,*,#4116,.F.);
#5462=ORIENTED_EDGE('',*,*,#4115,.T.);
#5463=ORIENTED_EDGE('',*,*,#4117,.F.);
#5464=ORIENTED_EDGE('',*,*,#4118,.F.);
#5465=ORIENTED_EDGE('',*,*,#4119,.F.);
#5466=ORIENTED_EDGE('',*,*,#4118,.T.);
#5467=ORIENTED_EDGE('',*,*,#4120,.F.);
#5468=ORIENTED_EDGE('',*,*,#4121,.F.);
#5469=ORIENTED_EDGE('',*,*,#4122,.F.);
#5470=ORIENTED_EDGE('',*,*,#4121,.T.);
#5471=ORIENTED_EDGE('',*,*,#4123,.F.);
#5472=ORIENTED_EDGE('',*,*,#4124,.F.);
#5473=ORIENTED_EDGE('',*,*,#4125,.F.);
#5474=ORIENTED_EDGE('',*,*,#4124,.T.);
#5475=ORIENTED_EDGE('',*,*,#4126,.F.);
#5476=ORIENTED_EDGE('',*,*,#4127,.F.);
#5477=ORIENTED_EDGE('',*,*,#4128,.F.);
#5478=ORIENTED_EDGE('',*,*,#4127,.T.);
#5479=ORIENTED_EDGE('',*,*,#4129,.F.);
#5480=ORIENTED_EDGE('',*,*,#4130,.F.);
#5481=ORIENTED_EDGE('',*,*,#4131,.F.);
#5482=ORIENTED_EDGE('',*,*,#4130,.T.);
#5483=ORIENTED_EDGE('',*,*,#4132,.F.);
#5484=ORIENTED_EDGE('',*,*,#4133,.F.);
#5485=ORIENTED_EDGE('',*,*,#4134,.F.);
#5486=ORIENTED_EDGE('',*,*,#4133,.T.);
#5487=ORIENTED_EDGE('',*,*,#4135,.F.);
#5488=ORIENTED_EDGE('',*,*,#4136,.F.);
#5489=ORIENTED_EDGE('',*,*,#4137,.F.);
#5490=ORIENTED_EDGE('',*,*,#4136,.T.);
#5491=ORIENTED_EDGE('',*,*,#4138,.F.);
#5492=ORIENTED_EDGE('',*,*,#3996,.F.);
#5493=ORIENTED_EDGE('',*,*,#4138,.T.);
#5494=ORIENTED_EDGE('',*,*,#4135,.T.);
#5495=ORIENTED_EDGE('',*,*,#4132,.T.);
#5496=ORIENTED_EDGE('',*,*,#4129,.T.);
#5497=ORIENTED_EDGE('',*,*,#4126,.T.);
#5498=ORIENTED_EDGE('',*,*,#4123,.T.);
#5499=ORIENTED_EDGE('',*,*,#4120,.T.);
#5500=ORIENTED_EDGE('',*,*,#4117,.T.);
#5501=ORIENTED_EDGE('',*,*,#4114,.T.);
#5502=ORIENTED_EDGE('',*,*,#4111,.T.);
#5503=ORIENTED_EDGE('',*,*,#4108,.T.);
#5504=ORIENTED_EDGE('',*,*,#4105,.T.);
#5505=ORIENTED_EDGE('',*,*,#4102,.T.);
#5506=ORIENTED_EDGE('',*,*,#4099,.T.);
#5507=ORIENTED_EDGE('',*,*,#4096,.T.);
#5508=ORIENTED_EDGE('',*,*,#4093,.T.);
#5509=ORIENTED_EDGE('',*,*,#4090,.T.);
#5510=ORIENTED_EDGE('',*,*,#4087,.T.);
#5511=ORIENTED_EDGE('',*,*,#4084,.T.);
#5512=ORIENTED_EDGE('',*,*,#4081,.T.);
#5513=ORIENTED_EDGE('',*,*,#4078,.T.);
#5514=ORIENTED_EDGE('',*,*,#4075,.T.);
#5515=ORIENTED_EDGE('',*,*,#4072,.T.);
#5516=ORIENTED_EDGE('',*,*,#4069,.T.);
#5517=ORIENTED_EDGE('',*,*,#4066,.T.);
#5518=ORIENTED_EDGE('',*,*,#4063,.T.);
#5519=ORIENTED_EDGE('',*,*,#4060,.T.);
#5520=ORIENTED_EDGE('',*,*,#4057,.T.);
#5521=ORIENTED_EDGE('',*,*,#4054,.T.);
#5522=ORIENTED_EDGE('',*,*,#4051,.T.);
#5523=ORIENTED_EDGE('',*,*,#4048,.T.);
#5524=ORIENTED_EDGE('',*,*,#4045,.T.);
#5525=ORIENTED_EDGE('',*,*,#4042,.T.);
#5526=ORIENTED_EDGE('',*,*,#4039,.T.);
#5527=ORIENTED_EDGE('',*,*,#4036,.T.);
#5528=ORIENTED_EDGE('',*,*,#4033,.T.);
#5529=ORIENTED_EDGE('',*,*,#4030,.T.);
#5530=ORIENTED_EDGE('',*,*,#4027,.T.);
#5531=ORIENTED_EDGE('',*,*,#4024,.T.);
#5532=ORIENTED_EDGE('',*,*,#4021,.T.);
#5533=ORIENTED_EDGE('',*,*,#4018,.T.);
#5534=ORIENTED_EDGE('',*,*,#4015,.T.);
#5535=ORIENTED_EDGE('',*,*,#4012,.T.);
#5536=ORIENTED_EDGE('',*,*,#4009,.T.);
#5537=ORIENTED_EDGE('',*,*,#4006,.T.);
#5538=ORIENTED_EDGE('',*,*,#4003,.T.);
#5539=ORIENTED_EDGE('',*,*,#4000,.T.);
#5540=ORIENTED_EDGE('',*,*,#3997,.T.);
#5541=ORIENTED_EDGE('',*,*,#3991,.T.);
#5542=ORIENTED_EDGE('',*,*,#4137,.T.);
#5543=ORIENTED_EDGE('',*,*,#3995,.T.);
#5544=ORIENTED_EDGE('',*,*,#3999,.T.);
#5545=ORIENTED_EDGE('',*,*,#4002,.T.);
#5546=ORIENTED_EDGE('',*,*,#4005,.T.);
#5547=ORIENTED_EDGE('',*,*,#4008,.T.);
#5548=ORIENTED_EDGE('',*,*,#4011,.T.);
#5549=ORIENTED_EDGE('',*,*,#4014,.T.);
#5550=ORIENTED_EDGE('',*,*,#4017,.T.);
#5551=ORIENTED_EDGE('',*,*,#4020,.T.);
#5552=ORIENTED_EDGE('',*,*,#4023,.T.);
#5553=ORIENTED_EDGE('',*,*,#4026,.T.);
#5554=ORIENTED_EDGE('',*,*,#4029,.T.);
#5555=ORIENTED_EDGE('',*,*,#4032,.T.);
#5556=ORIENTED_EDGE('',*,*,#4035,.T.);
#5557=ORIENTED_EDGE('',*,*,#4038,.T.);
#5558=ORIENTED_EDGE('',*,*,#4041,.T.);
#5559=ORIENTED_EDGE('',*,*,#4044,.T.);
#5560=ORIENTED_EDGE('',*,*,#4047,.T.);
#5561=ORIENTED_EDGE('',*,*,#4050,.T.);
#5562=ORIENTED_EDGE('',*,*,#4053,.T.);
#5563=ORIENTED_EDGE('',*,*,#4056,.T.);
#5564=ORIENTED_EDGE('',*,*,#4059,.T.);
#5565=ORIENTED_EDGE('',*,*,#4062,.T.);
#5566=ORIENTED_EDGE('',*,*,#4065,.T.);
#5567=ORIENTED_EDGE('',*,*,#4068,.T.);
#5568=ORIENTED_EDGE('',*,*,#4071,.T.);
#5569=ORIENTED_EDGE('',*,*,#4074,.T.);
#5570=ORIENTED_EDGE('',*,*,#4077,.T.);
#5571=ORIENTED_EDGE('',*,*,#4080,.T.);
#5572=ORIENTED_EDGE('',*,*,#4083,.T.);
#5573=ORIENTED_EDGE('',*,*,#4086,.T.);
#5574=ORIENTED_EDGE('',*,*,#4089,.T.);
#5575=ORIENTED_EDGE('',*,*,#4092,.T.);
#5576=ORIENTED_EDGE('',*,*,#4095,.T.);
#5577=ORIENTED_EDGE('',*,*,#4098,.T.);
#5578=ORIENTED_EDGE('',*,*,#4101,.T.);
#5579=ORIENTED_EDGE('',*,*,#4104,.T.);
#5580=ORIENTED_EDGE('',*,*,#4107,.T.);
#5581=ORIENTED_EDGE('',*,*,#4110,.T.);
#5582=ORIENTED_EDGE('',*,*,#4113,.T.);
#5583=ORIENTED_EDGE('',*,*,#4116,.T.);
#5584=ORIENTED_EDGE('',*,*,#4119,.T.);
#5585=ORIENTED_EDGE('',*,*,#4122,.T.);
#5586=ORIENTED_EDGE('',*,*,#4125,.T.);
#5587=ORIENTED_EDGE('',*,*,#4128,.T.);
#5588=ORIENTED_EDGE('',*,*,#4131,.T.);
#5589=ORIENTED_EDGE('',*,*,#4134,.T.);
#5590=ORIENTED_EDGE('',*,*,#3993,.T.);
#5591=ORIENTED_EDGE('',*,*,#4139,.F.);
#5592=ORIENTED_EDGE('',*,*,#4140,.T.);
#5593=ORIENTED_EDGE('',*,*,#4141,.F.);
#5594=ORIENTED_EDGE('',*,*,#4140,.F.);
#5595=ORIENTED_EDGE('',*,*,#4142,.F.);
#5596=ORIENTED_EDGE('',*,*,#4143,.T.);
#5597=ORIENTED_EDGE('',*,*,#4144,.F.);
#5598=ORIENTED_EDGE('',*,*,#4145,.F.);
#5599=ORIENTED_EDGE('',*,*,#4146,.T.);
#5600=ORIENTED_EDGE('',*,*,#4147,.T.);
#5601=ORIENTED_EDGE('',*,*,#4146,.F.);
#5602=ORIENTED_EDGE('',*,*,#4148,.F.);
#5603=ORIENTED_EDGE('',*,*,#4149,.F.);
#5604=ORIENTED_EDGE('',*,*,#4143,.F.);
#5605=ORIENTED_EDGE('',*,*,#4147,.F.);
#5606=ORIENTED_EDGE('',*,*,#4150,.F.);
#5607=ORIENTED_EDGE('',*,*,#4148,.T.);
#5608=ORIENTED_EDGE('',*,*,#4145,.T.);
#5609=ORIENTED_EDGE('',*,*,#4151,.F.);
#5610=ORIENTED_EDGE('',*,*,#4152,.T.);
#5611=ORIENTED_EDGE('',*,*,#4153,.T.);
#5612=ORIENTED_EDGE('',*,*,#4154,.T.);
#5613=ORIENTED_EDGE('',*,*,#4155,.F.);
#5614=ORIENTED_EDGE('',*,*,#4139,.T.);
#5615=ORIENTED_EDGE('',*,*,#4156,.F.);
#5616=ORIENTED_EDGE('',*,*,#4157,.F.);
#5617=ORIENTED_EDGE('',*,*,#4154,.F.);
#5618=ORIENTED_EDGE('',*,*,#4158,.T.);
#5619=ORIENTED_EDGE('',*,*,#4159,.F.);
#5620=ORIENTED_EDGE('',*,*,#4160,.F.);
#5621=ORIENTED_EDGE('',*,*,#4159,.T.);
#5622=ORIENTED_EDGE('',*,*,#4161,.T.);
#5623=ORIENTED_EDGE('',*,*,#4162,.T.);
#5624=ORIENTED_EDGE('',*,*,#4141,.T.);
#5625=ORIENTED_EDGE('',*,*,#4163,.F.);
#5626=ORIENTED_EDGE('',*,*,#4162,.F.);
#5627=ORIENTED_EDGE('',*,*,#4164,.F.);
#5628=ORIENTED_EDGE('',*,*,#4152,.F.);
#5629=ORIENTED_EDGE('',*,*,#4153,.F.);
#5630=ORIENTED_EDGE('',*,*,#4164,.T.);
#5631=ORIENTED_EDGE('',*,*,#4161,.F.);
#5632=ORIENTED_EDGE('',*,*,#4158,.F.);
#5633=ORIENTED_EDGE('',*,*,#4165,.F.);
#5634=ORIENTED_EDGE('',*,*,#4166,.T.);
#5635=ORIENTED_EDGE('',*,*,#4155,.T.);
#5636=ORIENTED_EDGE('',*,*,#4157,.T.);
#5637=ORIENTED_EDGE('',*,*,#4160,.T.);
#5638=ORIENTED_EDGE('',*,*,#4163,.T.);
#5639=ORIENTED_EDGE('',*,*,#4151,.T.);
#5640=ORIENTED_EDGE('',*,*,#4166,.F.);
#5641=ORIENTED_EDGE('',*,*,#4167,.F.);
#5642=ORIENTED_EDGE('',*,*,#4168,.T.);
#5643=ORIENTED_EDGE('',*,*,#4156,.T.);
#5644=ORIENTED_EDGE('',*,*,#4168,.F.);
#5645=ORIENTED_EDGE('',*,*,#4149,.T.);
#5646=ORIENTED_EDGE('',*,*,#4150,.T.);
#5647=ORIENTED_EDGE('',*,*,#4144,.T.);
#5648=ORIENTED_EDGE('',*,*,#4142,.T.);
#5649=ORIENTED_EDGE('',*,*,#4165,.T.);
#5650=ORIENTED_EDGE('',*,*,#4167,.T.);
#5651=ORIENTED_EDGE('',*,*,#4169,.F.);
#5652=ORIENTED_EDGE('',*,*,#4170,.T.);
#5653=ORIENTED_EDGE('',*,*,#4171,.F.);
#5654=ORIENTED_EDGE('',*,*,#4170,.F.);
#5655=ORIENTED_EDGE('',*,*,#4169,.T.);
#5656=ORIENTED_EDGE('',*,*,#4172,.F.);
#5657=ORIENTED_EDGE('',*,*,#4173,.T.);
#5658=ORIENTED_EDGE('',*,*,#4174,.T.);
#5659=ORIENTED_EDGE('',*,*,#4173,.F.);
#5660=ORIENTED_EDGE('',*,*,#4172,.T.);
#5661=ORIENTED_EDGE('',*,*,#4171,.T.);
#5662=ORIENTED_EDGE('',*,*,#4174,.F.);
#5663=ORIENTED_EDGE('',*,*,#4175,.F.);
#5664=ORIENTED_EDGE('',*,*,#4176,.T.);
#5665=ORIENTED_EDGE('',*,*,#4177,.T.);
#5666=ORIENTED_EDGE('',*,*,#4178,.F.);
#5667=ORIENTED_EDGE('',*,*,#4179,.F.);
#5668=ORIENTED_EDGE('',*,*,#4180,.T.);
#5669=ORIENTED_EDGE('',*,*,#4181,.T.);
#5670=ORIENTED_EDGE('',*,*,#4176,.F.);
#5671=ORIENTED_EDGE('',*,*,#4182,.F.);
#5672=ORIENTED_EDGE('',*,*,#4183,.T.);
#5673=ORIENTED_EDGE('',*,*,#4184,.T.);
#5674=ORIENTED_EDGE('',*,*,#4180,.F.);
#5675=ORIENTED_EDGE('',*,*,#4185,.F.);
#5676=ORIENTED_EDGE('',*,*,#4186,.T.);
#5677=ORIENTED_EDGE('',*,*,#4187,.T.);
#5678=ORIENTED_EDGE('',*,*,#4183,.F.);
#5679=ORIENTED_EDGE('',*,*,#4188,.F.);
#5680=ORIENTED_EDGE('',*,*,#4189,.T.);
#5681=ORIENTED_EDGE('',*,*,#4190,.T.);
#5682=ORIENTED_EDGE('',*,*,#4186,.F.);
#5683=ORIENTED_EDGE('',*,*,#4191,.F.);
#5684=ORIENTED_EDGE('',*,*,#4178,.T.);
#5685=ORIENTED_EDGE('',*,*,#4192,.T.);
#5686=ORIENTED_EDGE('',*,*,#4189,.F.);
#5687=ORIENTED_EDGE('',*,*,#4192,.F.);
#5688=ORIENTED_EDGE('',*,*,#4177,.F.);
#5689=ORIENTED_EDGE('',*,*,#4181,.F.);
#5690=ORIENTED_EDGE('',*,*,#4184,.F.);
#5691=ORIENTED_EDGE('',*,*,#4187,.F.);
#5692=ORIENTED_EDGE('',*,*,#4190,.F.);
#5693=ORIENTED_EDGE('',*,*,#4193,.F.);
#5694=ORIENTED_EDGE('',*,*,#4175,.T.);
#5695=ORIENTED_EDGE('',*,*,#4191,.T.);
#5696=ORIENTED_EDGE('',*,*,#4188,.T.);
#5697=ORIENTED_EDGE('',*,*,#4185,.T.);
#5698=ORIENTED_EDGE('',*,*,#4182,.T.);
#5699=ORIENTED_EDGE('',*,*,#4179,.T.);
#5700=ORIENTED_EDGE('',*,*,#4194,.F.);
#5701=ORIENTED_EDGE('',*,*,#4195,.T.);
#5702=ORIENTED_EDGE('',*,*,#4193,.T.);
#5703=ORIENTED_EDGE('',*,*,#4195,.F.);
#5704=ORIENTED_EDGE('',*,*,#4196,.F.);
#5705=ORIENTED_EDGE('',*,*,#4197,.T.);
#5706=ORIENTED_EDGE('',*,*,#4194,.T.);
#5707=ORIENTED_EDGE('',*,*,#4197,.F.);
#5708=ORIENTED_EDGE('',*,*,#4198,.F.);
#5709=ORIENTED_EDGE('',*,*,#4199,.T.);
#5710=ORIENTED_EDGE('',*,*,#4196,.T.);
#5711=ORIENTED_EDGE('',*,*,#4199,.F.);
#5712=ORIENTED_EDGE('',*,*,#4198,.T.);
#5713=ORIENTED_EDGE('',*,*,#4200,.F.);
#5714=ORIENTED_EDGE('',*,*,#4201,.F.);
#5715=ORIENTED_EDGE('',*,*,#4202,.T.);
#5716=ORIENTED_EDGE('',*,*,#4200,.T.);
#5717=ORIENTED_EDGE('',*,*,#4202,.F.);
#5718=ORIENTED_EDGE('',*,*,#4203,.F.);
#5719=ORIENTED_EDGE('',*,*,#4204,.T.);
#5720=ORIENTED_EDGE('',*,*,#4201,.T.);
#5721=ORIENTED_EDGE('',*,*,#4204,.F.);
#5722=ORIENTED_EDGE('',*,*,#4205,.F.);
#5723=ORIENTED_EDGE('',*,*,#4206,.T.);
#5724=ORIENTED_EDGE('',*,*,#4203,.T.);
#5725=ORIENTED_EDGE('',*,*,#4206,.F.);
#5726=ORIENTED_EDGE('',*,*,#4205,.T.);
#5727=ORIENTED_EDGE('',*,*,#4207,.F.);
#5728=ORIENTED_EDGE('',*,*,#4208,.F.);
#5729=ORIENTED_EDGE('',*,*,#4209,.T.);
#5730=ORIENTED_EDGE('',*,*,#4207,.T.);
#5731=ORIENTED_EDGE('',*,*,#4209,.F.);
#5732=ORIENTED_EDGE('',*,*,#4210,.F.);
#5733=ORIENTED_EDGE('',*,*,#4211,.T.);
#5734=ORIENTED_EDGE('',*,*,#4208,.T.);
#5735=ORIENTED_EDGE('',*,*,#4211,.F.);
#5736=ORIENTED_EDGE('',*,*,#4212,.F.);
#5737=ORIENTED_EDGE('',*,*,#4213,.T.);
#5738=ORIENTED_EDGE('',*,*,#4210,.T.);
#5739=ORIENTED_EDGE('',*,*,#4213,.F.);
#5740=ORIENTED_EDGE('',*,*,#4212,.T.);
#5741=ORIENTED_EDGE('',*,*,#4214,.T.);
#5742=ORIENTED_EDGE('',*,*,#4215,.T.);
#5743=ORIENTED_EDGE('',*,*,#4216,.T.);
#5744=ORIENTED_EDGE('',*,*,#4217,.F.);
#5745=ORIENTED_EDGE('',*,*,#4218,.T.);
#5746=ORIENTED_EDGE('',*,*,#4219,.T.);
#5747=ORIENTED_EDGE('',*,*,#4220,.T.);
#5748=ORIENTED_EDGE('',*,*,#4215,.F.);
#5749=ORIENTED_EDGE('',*,*,#4221,.T.);
#5750=ORIENTED_EDGE('',*,*,#4222,.T.);
#5751=ORIENTED_EDGE('',*,*,#4223,.T.);
#5752=ORIENTED_EDGE('',*,*,#4219,.F.);
#5753=ORIENTED_EDGE('',*,*,#4224,.T.);
#5754=ORIENTED_EDGE('',*,*,#4225,.T.);
#5755=ORIENTED_EDGE('',*,*,#4226,.T.);
#5756=ORIENTED_EDGE('',*,*,#4222,.F.);
#5757=ORIENTED_EDGE('',*,*,#4227,.T.);
#5758=ORIENTED_EDGE('',*,*,#4228,.T.);
#5759=ORIENTED_EDGE('',*,*,#4229,.T.);
#5760=ORIENTED_EDGE('',*,*,#4225,.F.);
#5761=ORIENTED_EDGE('',*,*,#4230,.T.);
#5762=ORIENTED_EDGE('',*,*,#4217,.T.);
#5763=ORIENTED_EDGE('',*,*,#4231,.T.);
#5764=ORIENTED_EDGE('',*,*,#4228,.F.);
#5765=ORIENTED_EDGE('',*,*,#4230,.F.);
#5766=ORIENTED_EDGE('',*,*,#4227,.F.);
#5767=ORIENTED_EDGE('',*,*,#4224,.F.);
#5768=ORIENTED_EDGE('',*,*,#4221,.F.);
#5769=ORIENTED_EDGE('',*,*,#4218,.F.);
#5770=ORIENTED_EDGE('',*,*,#4214,.F.);
#5771=ORIENTED_EDGE('',*,*,#4231,.F.);
#5772=ORIENTED_EDGE('',*,*,#4216,.F.);
#5773=ORIENTED_EDGE('',*,*,#4220,.F.);
#5774=ORIENTED_EDGE('',*,*,#4223,.F.);
#5775=ORIENTED_EDGE('',*,*,#4226,.F.);
#5776=ORIENTED_EDGE('',*,*,#4229,.F.);
#5777=ORIENTED_EDGE('',*,*,#4232,.F.);
#5778=ORIENTED_EDGE('',*,*,#4233,.T.);
#5779=ORIENTED_EDGE('',*,*,#4234,.F.);
#5780=ORIENTED_EDGE('',*,*,#4233,.F.);
#5781=ORIENTED_EDGE('',*,*,#4235,.F.);
#5782=ORIENTED_EDGE('',*,*,#4236,.T.);
#5783=ORIENTED_EDGE('',*,*,#4237,.F.);
#5784=ORIENTED_EDGE('',*,*,#4238,.F.);
#5785=ORIENTED_EDGE('',*,*,#4235,.T.);
#5786=ORIENTED_EDGE('',*,*,#4239,.F.);
#5787=ORIENTED_EDGE('',*,*,#4240,.F.);
#5788=ORIENTED_EDGE('',*,*,#4241,.F.);
#5789=ORIENTED_EDGE('',*,*,#4238,.T.);
#5790=ORIENTED_EDGE('',*,*,#4242,.T.);
#5791=ORIENTED_EDGE('',*,*,#4243,.T.);
#5792=ORIENTED_EDGE('',*,*,#4239,.T.);
#5793=ORIENTED_EDGE('',*,*,#4234,.T.);
#5794=ORIENTED_EDGE('',*,*,#4244,.F.);
#5795=ORIENTED_EDGE('',*,*,#4240,.T.);
#5796=ORIENTED_EDGE('',*,*,#4243,.F.);
#5797=ORIENTED_EDGE('',*,*,#4245,.F.);
#5798=ORIENTED_EDGE('',*,*,#4237,.T.);
#5799=ORIENTED_EDGE('',*,*,#4246,.F.);
#5800=ORIENTED_EDGE('',*,*,#4245,.T.);
#5801=ORIENTED_EDGE('',*,*,#4242,.F.);
#5802=ORIENTED_EDGE('',*,*,#4241,.T.);
#5803=ORIENTED_EDGE('',*,*,#4244,.T.);
#5804=ORIENTED_EDGE('',*,*,#4246,.T.);
#5805=ORIENTED_EDGE('',*,*,#4236,.F.);
#5806=ORIENTED_EDGE('',*,*,#4232,.T.);
#5807=CYLINDRICAL_SURFACE('',#6682,0.210000000000001);
#5808=CYLINDRICAL_SURFACE('',#6685,0.21);
#5809=CYLINDRICAL_SURFACE('',#6688,0.21);
#5810=CYLINDRICAL_SURFACE('',#6691,0.21);
#5811=CYLINDRICAL_SURFACE('',#6694,0.21);
#5812=CYLINDRICAL_SURFACE('',#6697,0.21);
#5813=CYLINDRICAL_SURFACE('',#6700,0.21);
#5814=CYLINDRICAL_SURFACE('',#6703,0.21);
#5815=CYLINDRICAL_SURFACE('',#6706,0.21);
#5816=CYLINDRICAL_SURFACE('',#6709,0.21);
#5817=CYLINDRICAL_SURFACE('',#6733,0.475);
#5818=CYLINDRICAL_SURFACE('',#6738,0.475);
#5819=CYLINDRICAL_SURFACE('',#6743,0.275);
#5820=CYLINDRICAL_SURFACE('',#6745,0.275);
#5821=CYLINDRICAL_SURFACE('',#6747,0.475);
#5822=CYLINDRICAL_SURFACE('',#6752,0.475);
#5823=CYLINDRICAL_SURFACE('',#6757,0.275);
#5824=CYLINDRICAL_SURFACE('',#6759,0.275);
#5825=CYLINDRICAL_SURFACE('',#6761,0.34);
#5826=CYLINDRICAL_SURFACE('',#6764,0.34);
#5827=CYLINDRICAL_SURFACE('',#6774,0.425);
#5828=CYLINDRICAL_SURFACE('',#6777,0.645);
#5829=CYLINDRICAL_SURFACE('',#6783,0.425);
#5830=CYLINDRICAL_SURFACE('',#6786,0.645);
#5831=CYLINDRICAL_SURFACE('',#6792,0.475);
#5832=CYLINDRICAL_SURFACE('',#6797,0.475);
#5833=CYLINDRICAL_SURFACE('',#6802,0.275);
#5834=CYLINDRICAL_SURFACE('',#6804,0.275);
#5835=CYLINDRICAL_SURFACE('',#6806,0.475);
#5836=CYLINDRICAL_SURFACE('',#6811,0.475);
#5837=CYLINDRICAL_SURFACE('',#6816,0.275);
#5838=CYLINDRICAL_SURFACE('',#6818,0.275);
#5839=CYLINDRICAL_SURFACE('',#6820,0.34);
#5840=CYLINDRICAL_SURFACE('',#6823,0.34);
#5841=CYLINDRICAL_SURFACE('',#6833,0.425);
#5842=CYLINDRICAL_SURFACE('',#6836,0.645);
#5843=CYLINDRICAL_SURFACE('',#6842,0.425);
#5844=CYLINDRICAL_SURFACE('',#6845,0.645);
#5845=CYLINDRICAL_SURFACE('',#6851,0.275);
#5846=CYLINDRICAL_SURFACE('',#6854,0.275);
#5847=CYLINDRICAL_SURFACE('',#6857,0.305);
#5848=CYLINDRICAL_SURFACE('',#6872,0.165);
#5849=CYLINDRICAL_SURFACE('',#6879,0.6);
#5850=CYLINDRICAL_SURFACE('',#6882,0.3);
#5851=CYLINDRICAL_SURFACE('',#6886,0.305);
#5852=CYLINDRICAL_SURFACE('',#6889,0.5);
#5853=CYLINDRICAL_SURFACE('',#6895,0.225);
#5854=CYLINDRICAL_SURFACE('',#6898,0.6);
#5855=CYLINDRICAL_SURFACE('',#6911,0.164999999999999);
#5856=CYLINDRICAL_SURFACE('',#6922,2.05);
#5857=CYLINDRICAL_SURFACE('',#6925,2.05);
#5858=CYLINDRICAL_SURFACE('',#6943,2.8);
#5859=CYLINDRICAL_SURFACE('',#6953,0.65);
#5860=CYLINDRICAL_SURFACE('',#6955,0.65);
#5861=CYLINDRICAL_SURFACE('',#6963,1.8);
#5862=CYLINDRICAL_SURFACE('',#6972,0.25);
#5863=CYLINDRICAL_SURFACE('',#6973,0.25);
#5864=CYLINDRICAL_SURFACE('',#6974,1.65);
#5865=CYLINDRICAL_SURFACE('',#6977,0.25);
#5866=CYLINDRICAL_SURFACE('',#6978,0.25);
#5867=CYLINDRICAL_SURFACE('',#6979,0.25);
#5868=CYLINDRICAL_SURFACE('',#6980,0.25);
#5869=CYLINDRICAL_SURFACE('',#6985,1.75);
#5870=CYLINDRICAL_SURFACE('',#6989,1.);
#5871=CYLINDRICAL_SURFACE('',#6993,0.42);
#5872=CYLINDRICAL_SURFACE('',#6996,0.8);
#5873=CYLINDRICAL_SURFACE('',#7016,0.65);
#5874=CYLINDRICAL_SURFACE('',#7024,0.3933);
#5875=CYLINDRICAL_SURFACE('',#7040,0.35);
#5876=CYLINDRICAL_SURFACE('',#7048,0.1954);
#5877=CYLINDRICAL_SURFACE('',#7051,1.);
#5878=CYLINDRICAL_SURFACE('',#7059,0.21);
#5879=CYLINDRICAL_SURFACE('',#7063,1.005);
#5880=CYLINDRICAL_SURFACE('',#7066,1.5);
#5881=CYLINDRICAL_SURFACE('',#7074,0.21);
#5882=CYLINDRICAL_SURFACE('',#7078,1.005);
#5883=CYLINDRICAL_SURFACE('',#7081,1.5);
#5884=CYLINDRICAL_SURFACE('',#7087,3.6);
#5885=CYLINDRICAL_SURFACE('',#7090,4.);
#5886=CYLINDRICAL_SURFACE('',#7096,1.005);
#5887=CYLINDRICAL_SURFACE('',#7099,4.5);
#5888=CYLINDRICAL_SURFACE('',#7107,0.21);
#5889=CYLINDRICAL_SURFACE('',#7111,1.005);
#5890=CYLINDRICAL_SURFACE('',#7114,1.6);
#5891=CYLINDRICAL_SURFACE('',#7120,1.005);
#5892=CYLINDRICAL_SURFACE('',#7123,4.5);
#5893=CYLINDRICAL_SURFACE('',#7131,0.21);
#5894=CYLINDRICAL_SURFACE('',#7135,1.005);
#5895=CYLINDRICAL_SURFACE('',#7138,1.6);
#5896=CYLINDRICAL_SURFACE('',#7146,0.21);
#5897=CYLINDRICAL_SURFACE('',#7150,1.6);
#5898=CYLINDRICAL_SURFACE('',#7155,1.005);
#5899=CYLINDRICAL_SURFACE('',#7208,0.275);
#5900=CYLINDRICAL_SURFACE('',#7213,0.21);
#5901=CYLINDRICAL_SURFACE('',#7228,1.6);
#5902=CYLINDRICAL_SURFACE('',#7230,1.005);
#5903=CYLINDRICAL_SURFACE('',#7234,0.21);
#5904=CYLINDRICAL_SURFACE('',#7238,0.7);
#5905=CYLINDRICAL_SURFACE('',#7255,0.24505);
#5906=CYLINDRICAL_SURFACE('',#7265,0.425);
#5907=CYLINDRICAL_SURFACE('',#7273,0.24505);
#5908=CYLINDRICAL_SURFACE('',#7343,0.305);
#5909=CYLINDRICAL_SURFACE('',#7346,0.7);
#5910=ADVANCED_FACE('',(#840),#5807,.F.);
#5911=ADVANCED_FACE('',(#841),#5808,.F.);
#5912=ADVANCED_FACE('',(#842),#5809,.F.);
#5913=ADVANCED_FACE('',(#843),#5810,.F.);
#5914=ADVANCED_FACE('',(#844),#5811,.F.);
#5915=ADVANCED_FACE('',(#845),#5812,.F.);
#5916=ADVANCED_FACE('',(#846),#5813,.F.);
#5917=ADVANCED_FACE('',(#847),#5814,.F.);
#5918=ADVANCED_FACE('',(#848),#5815,.F.);
#5919=ADVANCED_FACE('',(#849),#5816,.F.);
#5920=ADVANCED_FACE('',(#850),#601,.T.);
#5921=ADVANCED_FACE('',(#851),#602,.T.);
#5922=ADVANCED_FACE('',(#852),#603,.T.);
#5923=ADVANCED_FACE('',(#853),#604,.T.);
#5924=ADVANCED_FACE('',(#854,#456,#457,#458,#459,#460,#461,#462,#463,#464,
#465),#605,.T.);
#5925=ADVANCED_FACE('',(#855,#466,#467,#468,#469,#470,#471,#472,#473,#474,
#475),#606,.F.);
#5926=ADVANCED_FACE('',(#856),#607,.T.);
#5927=ADVANCED_FACE('',(#857),#608,.T.);
#5928=ADVANCED_FACE('',(#858),#609,.T.);
#5929=ADVANCED_FACE('',(#859),#610,.T.);
#5930=ADVANCED_FACE('',(#860),#611,.T.);
#5931=ADVANCED_FACE('',(#861),#612,.F.);
#5932=ADVANCED_FACE('',(#862),#613,.T.);
#5933=ADVANCED_FACE('',(#863),#614,.T.);
#5934=ADVANCED_FACE('',(#864),#615,.T.);
#5935=ADVANCED_FACE('',(#865),#616,.T.);
#5936=ADVANCED_FACE('',(#866),#617,.T.);
#5937=ADVANCED_FACE('',(#867),#618,.F.);
#5938=ADVANCED_FACE('',(#868),#5817,.F.);
#5939=ADVANCED_FACE('',(#869,#476),#619,.T.);
#5940=ADVANCED_FACE('',(#870),#5818,.F.);
#5941=ADVANCED_FACE('',(#871,#477),#620,.T.);
#5942=ADVANCED_FACE('',(#872),#5819,.F.);
#5943=ADVANCED_FACE('',(#873),#5820,.F.);
#5944=ADVANCED_FACE('',(#874),#5821,.F.);
#5945=ADVANCED_FACE('',(#875,#478),#621,.T.);
#5946=ADVANCED_FACE('',(#876),#5822,.F.);
#5947=ADVANCED_FACE('',(#877,#479),#622,.T.);
#5948=ADVANCED_FACE('',(#878),#5823,.F.);
#5949=ADVANCED_FACE('',(#879),#5824,.F.);
#5950=ADVANCED_FACE('',(#880),#5825,.F.);
#5951=ADVANCED_FACE('',(#881),#5826,.F.);
#5952=ADVANCED_FACE('',(#882),#623,.T.);
#5953=ADVANCED_FACE('',(#883),#624,.T.);
#5954=ADVANCED_FACE('',(#884),#625,.T.);
#5955=ADVANCED_FACE('',(#885),#626,.T.);
#5956=ADVANCED_FACE('',(#886,#480,#481,#482,#483,#484,#485),#627,.T.);
#5957=ADVANCED_FACE('',(#887,#486,#487,#488,#489,#490,#491),#628,.F.);
#5958=ADVANCED_FACE('',(#888),#5827,.F.);
#5959=ADVANCED_FACE('',(#889),#5828,.T.);
#5960=ADVANCED_FACE('',(#890,#492),#629,.T.);
#5961=ADVANCED_FACE('',(#891,#493),#630,.F.);
#5962=ADVANCED_FACE('',(#892),#5829,.F.);
#5963=ADVANCED_FACE('',(#893),#5830,.T.);
#5964=ADVANCED_FACE('',(#894,#494),#631,.T.);
#5965=ADVANCED_FACE('',(#895,#495),#632,.F.);
#5966=ADVANCED_FACE('',(#896),#5831,.F.);
#5967=ADVANCED_FACE('',(#897,#496),#633,.T.);
#5968=ADVANCED_FACE('',(#898),#5832,.F.);
#5969=ADVANCED_FACE('',(#899,#497),#634,.T.);
#5970=ADVANCED_FACE('',(#900),#5833,.F.);
#5971=ADVANCED_FACE('',(#901),#5834,.F.);
#5972=ADVANCED_FACE('',(#902),#5835,.F.);
#5973=ADVANCED_FACE('',(#903,#498),#635,.T.);
#5974=ADVANCED_FACE('',(#904),#5836,.F.);
#5975=ADVANCED_FACE('',(#905,#499),#636,.T.);
#5976=ADVANCED_FACE('',(#906),#5837,.F.);
#5977=ADVANCED_FACE('',(#907),#5838,.F.);
#5978=ADVANCED_FACE('',(#908),#5839,.F.);
#5979=ADVANCED_FACE('',(#909),#5840,.F.);
#5980=ADVANCED_FACE('',(#910),#637,.T.);
#5981=ADVANCED_FACE('',(#911),#638,.T.);
#5982=ADVANCED_FACE('',(#912),#639,.T.);
#5983=ADVANCED_FACE('',(#913),#640,.T.);
#5984=ADVANCED_FACE('',(#914,#500,#501,#502,#503,#504,#505),#641,.T.);
#5985=ADVANCED_FACE('',(#915,#506,#507,#508,#509,#510,#511),#642,.F.);
#5986=ADVANCED_FACE('',(#916),#5841,.F.);
#5987=ADVANCED_FACE('',(#917),#5842,.T.);
#5988=ADVANCED_FACE('',(#918,#512),#643,.T.);
#5989=ADVANCED_FACE('',(#919,#513),#644,.F.);
#5990=ADVANCED_FACE('',(#920),#5843,.F.);
#5991=ADVANCED_FACE('',(#921),#5844,.T.);
#5992=ADVANCED_FACE('',(#922,#514),#645,.T.);
#5993=ADVANCED_FACE('',(#923,#515),#646,.F.);
#5994=ADVANCED_FACE('',(#924),#5845,.F.);
#5995=ADVANCED_FACE('',(#925),#5846,.F.);
#5996=ADVANCED_FACE('',(#926),#5847,.F.);
#5997=ADVANCED_FACE('',(#927,#516,#517,#518),#647,.T.);
#5998=ADVANCED_FACE('',(#928),#648,.T.);
#5999=ADVANCED_FACE('',(#929),#649,.T.);
#6000=ADVANCED_FACE('',(#930),#650,.T.);
#6001=ADVANCED_FACE('',(#931),#651,.F.);
#6002=ADVANCED_FACE('',(#932,#519),#652,.T.);
#6003=ADVANCED_FACE('',(#933),#653,.T.);
#6004=ADVANCED_FACE('',(#934,#520),#654,.T.);
#6005=ADVANCED_FACE('',(#935),#655,.T.);
#6006=ADVANCED_FACE('',(#936),#656,.T.);
#6007=ADVANCED_FACE('',(#937,#521,#522),#657,.F.);
#6008=ADVANCED_FACE('',(#938),#5848,.F.);
#6009=ADVANCED_FACE('',(#939),#658,.T.);
#6010=ADVANCED_FACE('',(#940,#523),#659,.T.);
#6011=ADVANCED_FACE('',(#941),#5849,.T.);
#6012=ADVANCED_FACE('',(#942),#660,.F.);
#6013=ADVANCED_FACE('',(#943),#5850,.T.);
#6014=ADVANCED_FACE('',(#944,#524),#661,.T.);
#6015=ADVANCED_FACE('',(#945),#5851,.F.);
#6016=ADVANCED_FACE('',(#946),#5852,.T.);
#6017=ADVANCED_FACE('',(#947,#525),#662,.T.);
#6018=ADVANCED_FACE('',(#948,#526),#663,.F.);
#6019=ADVANCED_FACE('',(#949),#5853,.F.);
#6020=ADVANCED_FACE('',(#950),#5854,.T.);
#6021=ADVANCED_FACE('',(#951,#527),#664,.T.);
#6022=ADVANCED_FACE('',(#952,#528),#665,.F.);
#6023=ADVANCED_FACE('',(#953),#666,.T.);
#6024=ADVANCED_FACE('',(#954),#667,.T.);
#6025=ADVANCED_FACE('',(#955),#668,.T.);
#6026=ADVANCED_FACE('',(#956),#669,.T.);
#6027=ADVANCED_FACE('',(#957),#670,.T.);
#6028=ADVANCED_FACE('',(#958),#671,.F.);
#6029=ADVANCED_FACE('',(#959),#5855,.F.);
#6030=ADVANCED_FACE('',(#960),#672,.T.);
#6031=ADVANCED_FACE('',(#961),#673,.T.);
#6032=ADVANCED_FACE('',(#962),#674,.T.);
#6033=ADVANCED_FACE('',(#963),#675,.T.);
#6034=ADVANCED_FACE('',(#964,#529),#676,.T.);
#6035=ADVANCED_FACE('',(#965,#530),#677,.F.);
#6036=ADVANCED_FACE('',(#966),#5856,.F.);
#6037=ADVANCED_FACE('',(#967),#5857,.F.);
#6038=ADVANCED_FACE('',(#968,#531,#532),#319,.F.);
#6039=ADVANCED_FACE('',(#969),#678,.T.);
#6040=ADVANCED_FACE('',(#970),#679,.T.);
#6041=ADVANCED_FACE('',(#971),#680,.T.);
#6042=ADVANCED_FACE('',(#972),#681,.T.);
#6043=ADVANCED_FACE('',(#973),#682,.T.);
#6044=ADVANCED_FACE('',(#974),#683,.T.);
#6045=ADVANCED_FACE('',(#975,#533,#534,#535),#684,.T.);
#6046=ADVANCED_FACE('',(#976),#5858,.T.);
#6047=ADVANCED_FACE('',(#977,#536),#685,.F.);
#6048=ADVANCED_FACE('',(#978,#537),#686,.T.);
#6049=ADVANCED_FACE('',(#979),#687,.F.);
#6050=ADVANCED_FACE('',(#980),#688,.F.);
#6051=ADVANCED_FACE('',(#981),#689,.F.);
#6052=ADVANCED_FACE('',(#982),#690,.F.);
#6053=ADVANCED_FACE('',(#983),#691,.F.);
#6054=ADVANCED_FACE('',(#984),#5859,.F.);
#6055=ADVANCED_FACE('',(#985),#5860,.F.);
#6056=ADVANCED_FACE('',(#986),#692,.T.);
#6057=ADVANCED_FACE('',(#987),#693,.T.);
#6058=ADVANCED_FACE('',(#988),#694,.T.);
#6059=ADVANCED_FACE('',(#989),#695,.T.);
#6060=ADVANCED_FACE('',(#990,#538,#539,#540),#696,.F.);
#6061=ADVANCED_FACE('',(#991),#5861,.F.);
#6062=ADVANCED_FACE('',(#992,#541),#697,.T.);
#6063=ADVANCED_FACE('',(#993,#542,#543),#320,.T.);
#6064=ADVANCED_FACE('',(#994,#544),#698,.T.);
#6065=ADVANCED_FACE('',(#995),#5862,.F.);
#6066=ADVANCED_FACE('',(#996),#5863,.F.);
#6067=ADVANCED_FACE('',(#997,#545,#546,#547,#548,#549,#550),#5864,.T.);
#6068=ADVANCED_FACE('',(#998),#5865,.F.);
#6069=ADVANCED_FACE('',(#999),#5866,.F.);
#6070=ADVANCED_FACE('',(#1000),#5867,.F.);
#6071=ADVANCED_FACE('',(#1001),#5868,.F.);
#6072=ADVANCED_FACE('',(#1002,#551),#699,.T.);
#6073=ADVANCED_FACE('',(#1003,#552),#700,.T.);
#6074=ADVANCED_FACE('',(#1004),#5869,.T.);
#6075=ADVANCED_FACE('',(#1005,#553),#701,.T.);
#6076=ADVANCED_FACE('',(#1006,#554,#555,#556,#557,#558,#559),#5870,.F.);
#6077=ADVANCED_FACE('',(#1007),#5871,.F.);
#6078=ADVANCED_FACE('',(#1008),#5872,.T.);
#6079=ADVANCED_FACE('',(#1009,#560),#702,.T.);
#6080=ADVANCED_FACE('',(#1010,#561),#703,.F.);
#6081=ADVANCED_FACE('',(#1011),#704,.F.);
#6082=ADVANCED_FACE('',(#1012),#705,.F.);
#6083=ADVANCED_FACE('',(#1013),#706,.F.);
#6084=ADVANCED_FACE('',(#1014),#707,.F.);
#6085=ADVANCED_FACE('',(#1015),#708,.F.);
#6086=ADVANCED_FACE('',(#1016),#709,.F.);
#6087=ADVANCED_FACE('',(#1017),#710,.F.);
#6088=ADVANCED_FACE('',(#1018),#711,.F.);
#6089=ADVANCED_FACE('',(#1019),#712,.F.);
#6090=ADVANCED_FACE('',(#1020),#713,.T.);
#6091=ADVANCED_FACE('',(#1021),#11,.T.);
#6092=ADVANCED_FACE('',(#1022),#5873,.T.);
#6093=ADVANCED_FACE('',(#1023),#12,.T.);
#6094=ADVANCED_FACE('',(#1024,#562),#714,.T.);
#6095=ADVANCED_FACE('',(#1025),#13,.T.);
#6096=ADVANCED_FACE('',(#1026),#5874,.T.);
#6097=ADVANCED_FACE('',(#1027),#715,.F.);
#6098=ADVANCED_FACE('',(#1028),#716,.F.);
#6099=ADVANCED_FACE('',(#1029),#717,.F.);
#6100=ADVANCED_FACE('',(#1030),#718,.F.);
#6101=ADVANCED_FACE('',(#1031),#719,.F.);
#6102=ADVANCED_FACE('',(#1032),#720,.F.);
#6103=ADVANCED_FACE('',(#1033),#721,.F.);
#6104=ADVANCED_FACE('',(#1034),#722,.F.);
#6105=ADVANCED_FACE('',(#1035),#723,.F.);
#6106=ADVANCED_FACE('',(#1036),#724,.T.);
#6107=ADVANCED_FACE('',(#1037),#14,.T.);
#6108=ADVANCED_FACE('',(#1038),#5875,.T.);
#6109=ADVANCED_FACE('',(#1039),#15,.T.);
#6110=ADVANCED_FACE('',(#1040,#563),#725,.T.);
#6111=ADVANCED_FACE('',(#1041),#16,.T.);
#6112=ADVANCED_FACE('',(#1042),#5876,.T.);
#6113=ADVANCED_FACE('',(#1043),#5877,.T.);
#6114=ADVANCED_FACE('',(#1044),#726,.T.);
#6115=ADVANCED_FACE('',(#1045),#727,.F.);
#6116=ADVANCED_FACE('',(#1046),#728,.T.);
#6117=ADVANCED_FACE('',(#1047),#5878,.F.);
#6118=ADVANCED_FACE('',(#1048),#729,.T.);
#6119=ADVANCED_FACE('',(#1049,#564),#5879,.F.);
#6120=ADVANCED_FACE('',(#1050,#565),#5880,.T.);
#6121=ADVANCED_FACE('',(#1051,#566),#730,.T.);
#6122=ADVANCED_FACE('',(#1052,#567),#731,.F.);
#6123=ADVANCED_FACE('',(#1053),#732,.T.);
#6124=ADVANCED_FACE('',(#1054),#5881,.F.);
#6125=ADVANCED_FACE('',(#1055),#733,.T.);
#6126=ADVANCED_FACE('',(#1056,#568),#5882,.F.);
#6127=ADVANCED_FACE('',(#1057,#569),#5883,.T.);
#6128=ADVANCED_FACE('',(#1058,#570),#734,.T.);
#6129=ADVANCED_FACE('',(#1059,#571),#735,.F.);
#6130=ADVANCED_FACE('',(#1060),#5884,.F.);
#6131=ADVANCED_FACE('',(#1061),#5885,.T.);
#6132=ADVANCED_FACE('',(#1062,#572),#736,.T.);
#6133=ADVANCED_FACE('',(#1063,#573),#737,.F.);
#6134=ADVANCED_FACE('',(#1064),#5886,.F.);
#6135=ADVANCED_FACE('',(#1065),#5887,.T.);
#6136=ADVANCED_FACE('',(#1066,#574),#738,.T.);
#6137=ADVANCED_FACE('',(#1067,#575),#739,.F.);
#6138=ADVANCED_FACE('',(#1068),#740,.T.);
#6139=ADVANCED_FACE('',(#1069),#5888,.F.);
#6140=ADVANCED_FACE('',(#1070),#741,.T.);
#6141=ADVANCED_FACE('',(#1071,#576),#5889,.F.);
#6142=ADVANCED_FACE('',(#1072,#577),#5890,.T.);
#6143=ADVANCED_FACE('',(#1073,#578),#742,.T.);
#6144=ADVANCED_FACE('',(#1074,#579),#743,.F.);
#6145=ADVANCED_FACE('',(#1075),#5891,.F.);
#6146=ADVANCED_FACE('',(#1076),#5892,.T.);
#6147=ADVANCED_FACE('',(#1077,#580),#744,.T.);
#6148=ADVANCED_FACE('',(#1078,#581),#745,.F.);
#6149=ADVANCED_FACE('',(#1079),#746,.T.);
#6150=ADVANCED_FACE('',(#1080),#5893,.F.);
#6151=ADVANCED_FACE('',(#1081),#747,.T.);
#6152=ADVANCED_FACE('',(#1082,#582),#5894,.F.);
#6153=ADVANCED_FACE('',(#1083,#583),#5895,.T.);
#6154=ADVANCED_FACE('',(#1084,#584),#748,.T.);
#6155=ADVANCED_FACE('',(#1085,#585),#749,.F.);
#6156=ADVANCED_FACE('',(#1086),#750,.T.);
#6157=ADVANCED_FACE('',(#1087),#5896,.F.);
#6158=ADVANCED_FACE('',(#1088),#751,.T.);
#6159=ADVANCED_FACE('',(#1089,#586),#5897,.T.);
#6160=ADVANCED_FACE('',(#1090,#587),#752,.T.);
#6161=ADVANCED_FACE('',(#1091,#588),#5898,.F.);
#6162=ADVANCED_FACE('',(#1092),#753,.T.);
#6163=ADVANCED_FACE('',(#1093),#754,.T.);
#6164=ADVANCED_FACE('',(#1094),#755,.T.);
#6165=ADVANCED_FACE('',(#1095),#756,.T.);
#6166=ADVANCED_FACE('',(#1096),#757,.T.);
#6167=ADVANCED_FACE('',(#1097),#758,.T.);
#6168=ADVANCED_FACE('',(#1098),#759,.T.);
#6169=ADVANCED_FACE('',(#1099),#760,.T.);
#6170=ADVANCED_FACE('',(#1100),#761,.T.);
#6171=ADVANCED_FACE('',(#1101),#762,.T.);
#6172=ADVANCED_FACE('',(#1102),#763,.T.);
#6173=ADVANCED_FACE('',(#1103),#764,.T.);
#6174=ADVANCED_FACE('',(#1104),#765,.T.);
#6175=ADVANCED_FACE('',(#1105),#766,.T.);
#6176=ADVANCED_FACE('',(#1106),#767,.T.);
#6177=ADVANCED_FACE('',(#1107),#768,.T.);
#6178=ADVANCED_FACE('',(#1108),#769,.T.);
#6179=ADVANCED_FACE('',(#1109),#770,.T.);
#6180=ADVANCED_FACE('',(#1110),#771,.T.);
#6181=ADVANCED_FACE('',(#1111),#772,.T.);
#6182=ADVANCED_FACE('',(#1112),#773,.T.);
#6183=ADVANCED_FACE('',(#1113),#774,.T.);
#6184=ADVANCED_FACE('',(#1114),#775,.T.);
#6185=ADVANCED_FACE('',(#1115),#776,.T.);
#6186=ADVANCED_FACE('',(#1116),#777,.T.);
#6187=ADVANCED_FACE('',(#1117),#778,.T.);
#6188=ADVANCED_FACE('',(#1118),#779,.T.);
#6189=ADVANCED_FACE('',(#1119),#780,.T.);
#6190=ADVANCED_FACE('',(#1120),#781,.T.);
#6191=ADVANCED_FACE('',(#1121),#782,.T.);
#6192=ADVANCED_FACE('',(#1122),#783,.T.);
#6193=ADVANCED_FACE('',(#1123),#784,.T.);
#6194=ADVANCED_FACE('',(#1124),#785,.T.);
#6195=ADVANCED_FACE('',(#1125),#786,.T.);
#6196=ADVANCED_FACE('',(#1126),#787,.T.);
#6197=ADVANCED_FACE('',(#1127),#788,.T.);
#6198=ADVANCED_FACE('',(#1128),#789,.T.);
#6199=ADVANCED_FACE('',(#1129),#790,.T.);
#6200=ADVANCED_FACE('',(#1130),#791,.T.);
#6201=ADVANCED_FACE('',(#1131),#792,.T.);
#6202=ADVANCED_FACE('',(#1132),#793,.T.);
#6203=ADVANCED_FACE('',(#1133),#794,.T.);
#6204=ADVANCED_FACE('',(#1134),#795,.T.);
#6205=ADVANCED_FACE('',(#1135),#796,.T.);
#6206=ADVANCED_FACE('',(#1136),#797,.T.);
#6207=ADVANCED_FACE('',(#1137),#798,.T.);
#6208=ADVANCED_FACE('',(#1138),#799,.T.);
#6209=ADVANCED_FACE('',(#1139),#800,.T.);
#6210=ADVANCED_FACE('',(#1140,#589),#801,.T.);
#6211=ADVANCED_FACE('',(#1141,#590),#802,.F.);
#6212=ADVANCED_FACE('',(#1142),#5899,.F.);
#6213=ADVANCED_FACE('',(#1143),#803,.T.);
#6214=ADVANCED_FACE('',(#1144),#5900,.F.);
#6215=ADVANCED_FACE('',(#1145),#804,.F.);
#6216=ADVANCED_FACE('',(#1146),#805,.T.);
#6217=ADVANCED_FACE('',(#1147,#591,#592),#806,.F.);
#6218=ADVANCED_FACE('',(#1148),#807,.T.);
#6219=ADVANCED_FACE('',(#1149,#593),#808,.T.);
#6220=ADVANCED_FACE('',(#1150),#809,.T.);
#6221=ADVANCED_FACE('',(#1151),#810,.T.);
#6222=ADVANCED_FACE('',(#1152),#5901,.T.);
#6223=ADVANCED_FACE('',(#1153,#594),#5902,.F.);
#6224=ADVANCED_FACE('',(#1154,#595),#811,.T.);
#6225=ADVANCED_FACE('',(#1155),#5903,.F.);
#6226=ADVANCED_FACE('',(#1156),#812,.T.);
#6227=ADVANCED_FACE('',(#1157),#5904,.T.);
#6228=ADVANCED_FACE('',(#1158,#596),#813,.T.);
#6229=ADVANCED_FACE('',(#1159),#814,.F.);
#6230=ADVANCED_FACE('',(#1160),#815,.F.);
#6231=ADVANCED_FACE('',(#1161),#816,.F.);
#6232=ADVANCED_FACE('',(#1162),#817,.F.);
#6233=ADVANCED_FACE('',(#1163),#818,.F.);
#6234=ADVANCED_FACE('',(#1164),#819,.F.);
#6235=ADVANCED_FACE('',(#1165),#820,.F.);
#6236=ADVANCED_FACE('',(#1166),#821,.F.);
#6237=ADVANCED_FACE('',(#1167,#597),#822,.T.);
#6238=ADVANCED_FACE('',(#1168),#17,.T.);
#6239=ADVANCED_FACE('',(#1169),#5905,.T.);
#6240=ADVANCED_FACE('',(#1170),#18,.T.);
#6241=ADVANCED_FACE('',(#1171),#823,.T.);
#6242=ADVANCED_FACE('',(#1172),#824,.T.);
#6243=ADVANCED_FACE('',(#1173),#19,.T.);
#6244=ADVANCED_FACE('',(#1174),#5906,.T.);
#6245=ADVANCED_FACE('',(#1175),#20,.T.);
#6246=ADVANCED_FACE('',(#1176,#598),#825,.T.);
#6247=ADVANCED_FACE('',(#1177),#21,.T.);
#6248=ADVANCED_FACE('',(#1178),#5907,.T.);
#6249=ADVANCED_FACE('',(#1179),#22,.T.);
#6250=ADVANCED_FACE('',(#1180),#826,.T.);
#6251=ADVANCED_FACE('',(#1181),#827,.F.);
#6252=ADVANCED_FACE('',(#1182),#828,.F.);
#6253=ADVANCED_FACE('',(#1183),#829,.F.);
#6254=ADVANCED_FACE('',(#1184),#830,.F.);
#6255=ADVANCED_FACE('',(#1185),#831,.F.);
#6256=ADVANCED_FACE('',(#1186),#832,.F.);
#6257=ADVANCED_FACE('',(#1187),#833,.F.);
#6258=ADVANCED_FACE('',(#1188),#834,.F.);
#6259=ADVANCED_FACE('',(#1189),#5908,.F.);
#6260=ADVANCED_FACE('',(#1190),#5909,.T.);
#6261=ADVANCED_FACE('',(#1191),#835,.T.);
#6262=ADVANCED_FACE('',(#1192,#599),#836,.T.);
#6263=ADVANCED_FACE('',(#1193),#837,.T.);
#6264=ADVANCED_FACE('',(#1194),#838,.T.);
#6265=ADVANCED_FACE('',(#1195,#600),#839,.F.);
#6266=CLOSED_SHELL('',(#5910,#5911,#5912,#5913,#5914,#5915,#5916,#5917,
#5918,#5919,#5920,#5921,#5922,#5923,#5924,#5925));
#6267=CLOSED_SHELL('',(#5926,#5927,#5928,#5929,#5930,#5931));
#6268=CLOSED_SHELL('',(#5932,#5933,#5934,#5935,#5936,#5937));
#6269=CLOSED_SHELL('',(#5938,#5939,#5940,#5941,#5942,#5943,#5944,#5945,
#5946,#5947,#5948,#5949,#5950,#5951,#5952,#5953,#5954,#5955,#5956,#5957));
#6270=CLOSED_SHELL('',(#5958,#5959,#5960,#5961));
#6271=CLOSED_SHELL('',(#5962,#5963,#5964,#5965));
#6272=CLOSED_SHELL('',(#5966,#5967,#5968,#5969,#5970,#5971,#5972,#5973,
#5974,#5975,#5976,#5977,#5978,#5979,#5980,#5981,#5982,#5983,#5984,#5985));
#6273=CLOSED_SHELL('',(#5986,#5987,#5988,#5989));
#6274=CLOSED_SHELL('',(#5990,#5991,#5992,#5993));
#6275=CLOSED_SHELL('',(#5994,#5995,#5996,#5997,#5998,#5999,#6000,#6001,
#6002,#6003,#6004,#6005,#6006,#6007));
#6276=CLOSED_SHELL('',(#6008,#6009,#6010,#6011,#6012,#6013,#6014));
#6277=CLOSED_SHELL('',(#6015,#6016,#6017,#6018));
#6278=CLOSED_SHELL('',(#6019,#6020,#6021,#6022));
#6279=CLOSED_SHELL('',(#6023,#6024,#6025,#6026,#6027,#6028));
#6280=CLOSED_SHELL('',(#6029,#6030,#6031,#6032,#6033,#6034,#6035));
#6281=CLOSED_SHELL('',(#6036,#6037,#6038,#6039,#6040,#6041,#6042,#6043,
#6044,#6045,#6046,#6047,#6048,#6049,#6050,#6051,#6052,#6053,#6054,#6055,
#6056,#6057,#6058,#6059,#6060));
#6282=CLOSED_SHELL('',(#6061,#6062,#6063,#6064));
#6283=CLOSED_SHELL('',(#6065,#6066,#6067,#6068,#6069,#6070,#6071,#6072,
#6073,#6074,#6075,#6076));
#6284=CLOSED_SHELL('',(#6077,#6078,#6079,#6080));
#6285=CLOSED_SHELL('',(#6081,#6082,#6083,#6084,#6085,#6086,#6087,#6088));
#6286=CLOSED_SHELL('',(#6089,#6090,#6091,#6092,#6093,#6094,#6095,#6096));
#6287=CLOSED_SHELL('',(#6097,#6098,#6099,#6100,#6101,#6102,#6103,#6104));
#6288=CLOSED_SHELL('',(#6105,#6106,#6107,#6108,#6109,#6110,#6111,#6112));
#6289=CLOSED_SHELL('',(#6113,#6114,#6115));
#6290=CLOSED_SHELL('',(#6116,#6117,#6118,#6119,#6120,#6121,#6122));
#6291=CLOSED_SHELL('',(#6123,#6124,#6125,#6126,#6127,#6128,#6129));
#6292=CLOSED_SHELL('',(#6130,#6131,#6132,#6133));
#6293=CLOSED_SHELL('',(#6134,#6135,#6136,#6137));
#6294=CLOSED_SHELL('',(#6138,#6139,#6140,#6141,#6142,#6143,#6144));
#6295=CLOSED_SHELL('',(#6145,#6146,#6147,#6148));
#6296=CLOSED_SHELL('',(#6149,#6150,#6151,#6152,#6153,#6154,#6155));
#6297=CLOSED_SHELL('',(#6156,#6157,#6158,#6159,#6160,#6161,#6162,#6163,
#6164,#6165,#6166,#6167,#6168,#6169,#6170,#6171,#6172,#6173,#6174,#6175,
#6176,#6177,#6178,#6179,#6180,#6181,#6182,#6183,#6184,#6185,#6186,#6187,
#6188,#6189,#6190,#6191,#6192,#6193,#6194,#6195,#6196,#6197,#6198,#6199,
#6200,#6201,#6202,#6203,#6204,#6205,#6206,#6207,#6208,#6209,#6210,#6211));
#6298=CLOSED_SHELL('',(#6212,#6213,#6214,#6215,#6216,#6217,#6218,#6219,
#6220,#6221,#6222,#6223,#6224));
#6299=CLOSED_SHELL('',(#6225,#6226,#6227,#6228,#6229));
#6300=CLOSED_SHELL('',(#6230,#6231,#6232,#6233,#6234,#6235,#6236,#6237,
#6238,#6239,#6240,#6241));
#6301=CLOSED_SHELL('',(#6242,#6243,#6244,#6245,#6246,#6247,#6248,#6249,
#6250));
#6302=CLOSED_SHELL('',(#6251,#6252,#6253,#6254,#6255,#6256,#6257,#6258));
#6303=CLOSED_SHELL('',(#6259,#6260,#6261,#6262,#6263,#6264,#6265));
#6304=DERIVED_UNIT_ELEMENT(#6372,1.);
#6305=DERIVED_UNIT_ELEMENT(#11803,-3.);
#6306=DERIVED_UNIT_ELEMENT(#6372,1.);
#6307=DERIVED_UNIT_ELEMENT(#11803,-3.);
#6308=DERIVED_UNIT_ELEMENT(#6372,1.);
#6309=DERIVED_UNIT_ELEMENT(#11803,-3.);
#6310=DERIVED_UNIT_ELEMENT(#6372,1.);
#6311=DERIVED_UNIT_ELEMENT(#11803,-3.);
#6312=DERIVED_UNIT_ELEMENT(#6372,1.);
#6313=DERIVED_UNIT_ELEMENT(#11803,-3.);
#6314=DERIVED_UNIT_ELEMENT(#6372,1.);
#6315=DERIVED_UNIT_ELEMENT(#11803,-3.);
#6316=DERIVED_UNIT_ELEMENT(#6372,1.);
#6317=DERIVED_UNIT_ELEMENT(#11803,-3.);
#6318=DERIVED_UNIT_ELEMENT(#6372,1.);
#6319=DERIVED_UNIT_ELEMENT(#11803,-3.);
#6320=DERIVED_UNIT_ELEMENT(#6372,1.);
#6321=DERIVED_UNIT_ELEMENT(#11803,-3.);
#6322=DERIVED_UNIT_ELEMENT(#6372,1.);
#6323=DERIVED_UNIT_ELEMENT(#11803,-3.);
#6324=DERIVED_UNIT_ELEMENT(#6372,1.);
#6325=DERIVED_UNIT_ELEMENT(#11803,-3.);
#6326=DERIVED_UNIT_ELEMENT(#6372,1.);
#6327=DERIVED_UNIT_ELEMENT(#11803,-3.);
#6328=DERIVED_UNIT_ELEMENT(#6372,1.);
#6329=DERIVED_UNIT_ELEMENT(#11803,-3.);
#6330=DERIVED_UNIT_ELEMENT(#6372,1.);
#6331=DERIVED_UNIT_ELEMENT(#11803,-3.);
#6332=DERIVED_UNIT_ELEMENT(#6372,1.);
#6333=DERIVED_UNIT_ELEMENT(#11803,-3.);
#6334=DERIVED_UNIT_ELEMENT(#6372,1.);
#6335=DERIVED_UNIT_ELEMENT(#11803,-3.);
#6336=DERIVED_UNIT_ELEMENT(#6372,1.);
#6337=DERIVED_UNIT_ELEMENT(#11803,-3.);
#6338=DERIVED_UNIT_ELEMENT(#6372,1.);
#6339=DERIVED_UNIT_ELEMENT(#11803,-3.);
#6340=DERIVED_UNIT_ELEMENT(#6372,1.);
#6341=DERIVED_UNIT_ELEMENT(#11803,-3.);
#6342=DERIVED_UNIT_ELEMENT(#6372,1.);
#6343=DERIVED_UNIT_ELEMENT(#11803,-3.);
#6344=DERIVED_UNIT_ELEMENT(#6372,1.);
#6345=DERIVED_UNIT_ELEMENT(#11803,-3.);
#6346=DERIVED_UNIT_ELEMENT(#6372,1.);
#6347=DERIVED_UNIT_ELEMENT(#11803,-3.);
#6348=DERIVED_UNIT_ELEMENT(#6372,1.);
#6349=DERIVED_UNIT_ELEMENT(#11803,-3.);
#6350=DERIVED_UNIT_ELEMENT(#6372,1.);
#6351=DERIVED_UNIT_ELEMENT(#11803,-3.);
#6352=DERIVED_UNIT_ELEMENT(#6372,1.);
#6353=DERIVED_UNIT_ELEMENT(#11803,-3.);
#6354=DERIVED_UNIT_ELEMENT(#6372,1.);
#6355=DERIVED_UNIT_ELEMENT(#11803,-3.);
#6356=DERIVED_UNIT_ELEMENT(#6372,1.);
#6357=DERIVED_UNIT_ELEMENT(#11803,-3.);
#6358=DERIVED_UNIT_ELEMENT(#6372,1.);
#6359=DERIVED_UNIT_ELEMENT(#11803,-3.);
#6360=DERIVED_UNIT_ELEMENT(#6372,1.);
#6361=DERIVED_UNIT_ELEMENT(#11803,-3.);
#6362=DERIVED_UNIT_ELEMENT(#6372,1.);
#6363=DERIVED_UNIT_ELEMENT(#11803,-3.);
#6364=DERIVED_UNIT_ELEMENT(#6372,1.);
#6365=DERIVED_UNIT_ELEMENT(#11803,-3.);
#6366=DERIVED_UNIT_ELEMENT(#6372,1.);
#6367=DERIVED_UNIT_ELEMENT(#11803,-3.);
#6368=DERIVED_UNIT_ELEMENT(#6372,1.);
#6369=DERIVED_UNIT_ELEMENT(#11803,-3.);
#6370=DERIVED_UNIT_ELEMENT(#6372,1.);
#6371=DERIVED_UNIT_ELEMENT(#11803,-3.);
#6372=(
MASS_UNIT()
NAMED_UNIT(*)
SI_UNIT(.KILO.,.GRAM.)
);
#6373=DERIVED_UNIT((#6304,#6305));
#6374=DERIVED_UNIT((#6306,#6307));
#6375=DERIVED_UNIT((#6308,#6309));
#6376=DERIVED_UNIT((#6310,#6311));
#6377=DERIVED_UNIT((#6312,#6313));
#6378=DERIVED_UNIT((#6314,#6315));
#6379=DERIVED_UNIT((#6316,#6317));
#6380=DERIVED_UNIT((#6318,#6319));
#6381=DERIVED_UNIT((#6320,#6321));
#6382=DERIVED_UNIT((#6322,#6323));
#6383=DERIVED_UNIT((#6324,#6325));
#6384=DERIVED_UNIT((#6326,#6327));
#6385=DERIVED_UNIT((#6328,#6329));
#6386=DERIVED_UNIT((#6330,#6331));
#6387=DERIVED_UNIT((#6332,#6333));
#6388=DERIVED_UNIT((#6334,#6335));
#6389=DERIVED_UNIT((#6336,#6337));
#6390=DERIVED_UNIT((#6338,#6339));
#6391=DERIVED_UNIT((#6340,#6341));
#6392=DERIVED_UNIT((#6342,#6343));
#6393=DERIVED_UNIT((#6344,#6345));
#6394=DERIVED_UNIT((#6346,#6347));
#6395=DERIVED_UNIT((#6348,#6349));
#6396=DERIVED_UNIT((#6350,#6351));
#6397=DERIVED_UNIT((#6352,#6353));
#6398=DERIVED_UNIT((#6354,#6355));
#6399=DERIVED_UNIT((#6356,#6357));
#6400=DERIVED_UNIT((#6358,#6359));
#6401=DERIVED_UNIT((#6360,#6361));
#6402=DERIVED_UNIT((#6362,#6363));
#6403=DERIVED_UNIT((#6364,#6365));
#6404=DERIVED_UNIT((#6366,#6367));
#6405=DERIVED_UNIT((#6368,#6369));
#6406=DERIVED_UNIT((#6370,#6371));
#6407=MEASURE_REPRESENTATION_ITEM('density measure',
POSITIVE_RATIO_MEASURE(7850.),#6373);
#6408=MEASURE_REPRESENTATION_ITEM('density measure',
POSITIVE_RATIO_MEASURE(7850.),#6374);
#6409=MEASURE_REPRESENTATION_ITEM('density measure',
POSITIVE_RATIO_MEASURE(7850.),#6375);
#6410=MEASURE_REPRESENTATION_ITEM('density measure',
POSITIVE_RATIO_MEASURE(7850.),#6376);
#6411=MEASURE_REPRESENTATION_ITEM('density measure',
POSITIVE_RATIO_MEASURE(7850.),#6377);
#6412=MEASURE_REPRESENTATION_ITEM('density measure',
POSITIVE_RATIO_MEASURE(7850.),#6378);
#6413=MEASURE_REPRESENTATION_ITEM('density measure',
POSITIVE_RATIO_MEASURE(7850.),#6379);
#6414=MEASURE_REPRESENTATION_ITEM('density measure',
POSITIVE_RATIO_MEASURE(7850.),#6380);
#6415=MEASURE_REPRESENTATION_ITEM('density measure',
POSITIVE_RATIO_MEASURE(7850.),#6381);
#6416=MEASURE_REPRESENTATION_ITEM('density measure',
POSITIVE_RATIO_MEASURE(7850.),#6382);
#6417=MEASURE_REPRESENTATION_ITEM('density measure',
POSITIVE_RATIO_MEASURE(7850.),#6383);
#6418=MEASURE_REPRESENTATION_ITEM('density measure',
POSITIVE_RATIO_MEASURE(7850.),#6384);
#6419=MEASURE_REPRESENTATION_ITEM('density measure',
POSITIVE_RATIO_MEASURE(7850.),#6385);
#6420=MEASURE_REPRESENTATION_ITEM('density measure',
POSITIVE_RATIO_MEASURE(7850.),#6386);
#6421=MEASURE_REPRESENTATION_ITEM('density measure',
POSITIVE_RATIO_MEASURE(7850.),#6387);
#6422=MEASURE_REPRESENTATION_ITEM('density measure',
POSITIVE_RATIO_MEASURE(7850.),#6388);
#6423=MEASURE_REPRESENTATION_ITEM('density measure',
POSITIVE_RATIO_MEASURE(7850.),#6389);
#6424=MEASURE_REPRESENTATION_ITEM('density measure',
POSITIVE_RATIO_MEASURE(7850.),#6390);
#6425=MEASURE_REPRESENTATION_ITEM('density measure',
POSITIVE_RATIO_MEASURE(7850.),#6391);
#6426=MEASURE_REPRESENTATION_ITEM('density measure',
POSITIVE_RATIO_MEASURE(7850.),#6392);
#6427=MEASURE_REPRESENTATION_ITEM('density measure',
POSITIVE_RATIO_MEASURE(7850.),#6393);
#6428=MEASURE_REPRESENTATION_ITEM('density measure',
POSITIVE_RATIO_MEASURE(7850.),#6394);
#6429=MEASURE_REPRESENTATION_ITEM('density measure',
POSITIVE_RATIO_MEASURE(7850.),#6395);
#6430=MEASURE_REPRESENTATION_ITEM('density measure',
POSITIVE_RATIO_MEASURE(7850.),#6396);
#6431=MEASURE_REPRESENTATION_ITEM('density measure',
POSITIVE_RATIO_MEASURE(7850.),#6397);
#6432=MEASURE_REPRESENTATION_ITEM('density measure',
POSITIVE_RATIO_MEASURE(7850.),#6398);
#6433=MEASURE_REPRESENTATION_ITEM('density measure',
POSITIVE_RATIO_MEASURE(7850.),#6399);
#6434=MEASURE_REPRESENTATION_ITEM('density measure',
POSITIVE_RATIO_MEASURE(7850.),#6400);
#6435=MEASURE_REPRESENTATION_ITEM('density measure',
POSITIVE_RATIO_MEASURE(7850.),#6401);
#6436=MEASURE_REPRESENTATION_ITEM('density measure',
POSITIVE_RATIO_MEASURE(7850.),#6402);
#6437=MEASURE_REPRESENTATION_ITEM('density measure',
POSITIVE_RATIO_MEASURE(7850.),#6403);
#6438=MEASURE_REPRESENTATION_ITEM('density measure',
POSITIVE_RATIO_MEASURE(7850.),#6404);
#6439=MEASURE_REPRESENTATION_ITEM('density measure',
POSITIVE_RATIO_MEASURE(7850.),#6405);
#6440=MEASURE_REPRESENTATION_ITEM('density measure',
POSITIVE_RATIO_MEASURE(7850.),#6406);
#6441=PROPERTY_DEFINITION_REPRESENTATION(#6611,#6509);
#6442=PROPERTY_DEFINITION_REPRESENTATION(#6612,#6510);
#6443=PROPERTY_DEFINITION_REPRESENTATION(#6613,#6511);
#6444=PROPERTY_DEFINITION_REPRESENTATION(#6614,#6512);
#6445=PROPERTY_DEFINITION_REPRESENTATION(#6615,#6513);
#6446=PROPERTY_DEFINITION_REPRESENTATION(#6616,#6514);
#6447=PROPERTY_DEFINITION_REPRESENTATION(#6617,#6515);
#6448=PROPERTY_DEFINITION_REPRESENTATION(#6618,#6516);
#6449=PROPERTY_DEFINITION_REPRESENTATION(#6619,#6517);
#6450=PROPERTY_DEFINITION_REPRESENTATION(#6620,#6518);
#6451=PROPERTY_DEFINITION_REPRESENTATION(#6621,#6519);
#6452=PROPERTY_DEFINITION_REPRESENTATION(#6622,#6520);
#6453=PROPERTY_DEFINITION_REPRESENTATION(#6623,#6521);
#6454=PROPERTY_DEFINITION_REPRESENTATION(#6624,#6522);
#6455=PROPERTY_DEFINITION_REPRESENTATION(#6625,#6523);
#6456=PROPERTY_DEFINITION_REPRESENTATION(#6626,#6524);
#6457=PROPERTY_DEFINITION_REPRESENTATION(#6627,#6525);
#6458=PROPERTY_DEFINITION_REPRESENTATION(#6628,#6526);
#6459=PROPERTY_DEFINITION_REPRESENTATION(#6629,#6527);
#6460=PROPERTY_DEFINITION_REPRESENTATION(#6630,#6528);
#6461=PROPERTY_DEFINITION_REPRESENTATION(#6631,#6529);
#6462=PROPERTY_DEFINITION_REPRESENTATION(#6632,#6530);
#6463=PROPERTY_DEFINITION_REPRESENTATION(#6633,#6531);
#6464=PROPERTY_DEFINITION_REPRESENTATION(#6634,#6532);
#6465=PROPERTY_DEFINITION_REPRESENTATION(#6635,#6533);
#6466=PROPERTY_DEFINITION_REPRESENTATION(#6636,#6534);
#6467=PROPERTY_DEFINITION_REPRESENTATION(#6637,#6535);
#6468=PROPERTY_DEFINITION_REPRESENTATION(#6638,#6536);
#6469=PROPERTY_DEFINITION_REPRESENTATION(#6639,#6537);
#6470=PROPERTY_DEFINITION_REPRESENTATION(#6640,#6538);
#6471=PROPERTY_DEFINITION_REPRESENTATION(#6641,#6539);
#6472=PROPERTY_DEFINITION_REPRESENTATION(#6642,#6540);
#6473=PROPERTY_DEFINITION_REPRESENTATION(#6643,#6541);
#6474=PROPERTY_DEFINITION_REPRESENTATION(#6644,#6542);
#6475=PROPERTY_DEFINITION_REPRESENTATION(#6645,#6543);
#6476=PROPERTY_DEFINITION_REPRESENTATION(#6646,#6544);
#6477=PROPERTY_DEFINITION_REPRESENTATION(#6647,#6545);
#6478=PROPERTY_DEFINITION_REPRESENTATION(#6648,#6546);
#6479=PROPERTY_DEFINITION_REPRESENTATION(#6649,#6547);
#6480=PROPERTY_DEFINITION_REPRESENTATION(#6650,#6548);
#6481=PROPERTY_DEFINITION_REPRESENTATION(#6651,#6549);
#6482=PROPERTY_DEFINITION_REPRESENTATION(#6652,#6550);
#6483=PROPERTY_DEFINITION_REPRESENTATION(#6653,#6551);
#6484=PROPERTY_DEFINITION_REPRESENTATION(#6654,#6552);
#6485=PROPERTY_DEFINITION_REPRESENTATION(#6655,#6553);
#6486=PROPERTY_DEFINITION_REPRESENTATION(#6656,#6554);
#6487=PROPERTY_DEFINITION_REPRESENTATION(#6657,#6555);
#6488=PROPERTY_DEFINITION_REPRESENTATION(#6658,#6556);
#6489=PROPERTY_DEFINITION_REPRESENTATION(#6659,#6557);
#6490=PROPERTY_DEFINITION_REPRESENTATION(#6660,#6558);
#6491=PROPERTY_DEFINITION_REPRESENTATION(#6661,#6559);
#6492=PROPERTY_DEFINITION_REPRESENTATION(#6662,#6560);
#6493=PROPERTY_DEFINITION_REPRESENTATION(#6663,#6561);
#6494=PROPERTY_DEFINITION_REPRESENTATION(#6664,#6562);
#6495=PROPERTY_DEFINITION_REPRESENTATION(#6665,#6563);
#6496=PROPERTY_DEFINITION_REPRESENTATION(#6666,#6564);
#6497=PROPERTY_DEFINITION_REPRESENTATION(#6667,#6565);
#6498=PROPERTY_DEFINITION_REPRESENTATION(#6668,#6566);
#6499=PROPERTY_DEFINITION_REPRESENTATION(#6669,#6567);
#6500=PROPERTY_DEFINITION_REPRESENTATION(#6670,#6568);
#6501=PROPERTY_DEFINITION_REPRESENTATION(#6671,#6569);
#6502=PROPERTY_DEFINITION_REPRESENTATION(#6672,#6570);
#6503=PROPERTY_DEFINITION_REPRESENTATION(#6673,#6571);
#6504=PROPERTY_DEFINITION_REPRESENTATION(#6674,#6572);
#6505=PROPERTY_DEFINITION_REPRESENTATION(#6675,#6573);
#6506=PROPERTY_DEFINITION_REPRESENTATION(#6676,#6574);
#6507=PROPERTY_DEFINITION_REPRESENTATION(#6677,#6575);
#6508=PROPERTY_DEFINITION_REPRESENTATION(#6678,#6576);
#6509=REPRESENTATION('material name',(#6577),#11764);
#6510=REPRESENTATION('density',(#6407),#11764);
#6511=REPRESENTATION('material name',(#6578),#11765);
#6512=REPRESENTATION('density',(#6408),#11765);
#6513=REPRESENTATION('material name',(#6579),#11766);
#6514=REPRESENTATION('density',(#6409),#11766);
#6515=REPRESENTATION('material name',(#6580),#11767);
#6516=REPRESENTATION('density',(#6410),#11767);
#6517=REPRESENTATION('material name',(#6581),#11768);
#6518=REPRESENTATION('density',(#6411),#11768);
#6519=REPRESENTATION('material name',(#6582),#11769);
#6520=REPRESENTATION('density',(#6412),#11769);
#6521=REPRESENTATION('material name',(#6583),#11770);
#6522=REPRESENTATION('density',(#6413),#11770);
#6523=REPRESENTATION('material name',(#6584),#11771);
#6524=REPRESENTATION('density',(#6414),#11771);
#6525=REPRESENTATION('material name',(#6585),#11772);
#6526=REPRESENTATION('density',(#6415),#11772);
#6527=REPRESENTATION('material name',(#6586),#11773);
#6528=REPRESENTATION('density',(#6416),#11773);
#6529=REPRESENTATION('material name',(#6587),#11774);
#6530=REPRESENTATION('density',(#6417),#11774);
#6531=REPRESENTATION('material name',(#6588),#11775);
#6532=REPRESENTATION('density',(#6418),#11775);
#6533=REPRESENTATION('material name',(#6589),#11776);
#6534=REPRESENTATION('density',(#6419),#11776);
#6535=REPRESENTATION('material name',(#6590),#11777);
#6536=REPRESENTATION('density',(#6420),#11777);
#6537=REPRESENTATION('material name',(#6591),#11778);
#6538=REPRESENTATION('density',(#6421),#11778);
#6539=REPRESENTATION('material name',(#6592),#11780);
#6540=REPRESENTATION('density',(#6422),#11780);
#6541=REPRESENTATION('material name',(#6593),#11781);
#6542=REPRESENTATION('density',(#6423),#11781);
#6543=REPRESENTATION('material name',(#6594),#11782);
#6544=REPRESENTATION('density',(#6424),#11782);
#6545=REPRESENTATION('material name',(#6595),#11783);
#6546=REPRESENTATION('density',(#6425),#11783);
#6547=REPRESENTATION('material name',(#6596),#11784);
#6548=REPRESENTATION('density',(#6426),#11784);
#6549=REPRESENTATION('material name',(#6597),#11786);
#6550=REPRESENTATION('density',(#6427),#11786);
#6551=REPRESENTATION('material name',(#6598),#11787);
#6552=REPRESENTATION('density',(#6428),#11787);
#6553=REPRESENTATION('material name',(#6599),#11788);
#6554=REPRESENTATION('density',(#6429),#11788);
#6555=REPRESENTATION('material name',(#6600),#11789);
#6556=REPRESENTATION('density',(#6430),#11789);
#6557=REPRESENTATION('material name',(#6601),#11790);
#6558=REPRESENTATION('density',(#6431),#11790);
#6559=REPRESENTATION('material name',(#6602),#11791);
#6560=REPRESENTATION('density',(#6432),#11791);
#6561=REPRESENTATION('material name',(#6603),#11792);
#6562=REPRESENTATION('density',(#6433),#11792);
#6563=REPRESENTATION('material name',(#6604),#11793);
#6564=REPRESENTATION('density',(#6434),#11793);
#6565=REPRESENTATION('material name',(#6605),#11794);
#6566=REPRESENTATION('density',(#6435),#11794);
#6567=REPRESENTATION('material name',(#6606),#11795);
#6568=REPRESENTATION('density',(#6436),#11795);
#6569=REPRESENTATION('material name',(#6607),#11796);
#6570=REPRESENTATION('density',(#6437),#11796);
#6571=REPRESENTATION('material name',(#6608),#11797);
#6572=REPRESENTATION('density',(#6438),#11797);
#6573=REPRESENTATION('material name',(#6609),#11798);
#6574=REPRESENTATION('density',(#6439),#11798);
#6575=REPRESENTATION('material name',(#6610),#11800);
#6576=REPRESENTATION('density',(#6440),#11800);
#6577=DESCRIPTIVE_REPRESENTATION_ITEM('Steel','Steel');
#6578=DESCRIPTIVE_REPRESENTATION_ITEM('Steel','Steel');
#6579=DESCRIPTIVE_REPRESENTATION_ITEM('Steel','Steel');
#6580=DESCRIPTIVE_REPRESENTATION_ITEM('Steel','Steel');
#6581=DESCRIPTIVE_REPRESENTATION_ITEM('Steel','Steel');
#6582=DESCRIPTIVE_REPRESENTATION_ITEM('Steel','Steel');
#6583=DESCRIPTIVE_REPRESENTATION_ITEM('Steel','Steel');
#6584=DESCRIPTIVE_REPRESENTATION_ITEM('Steel','Steel');
#6585=DESCRIPTIVE_REPRESENTATION_ITEM('Steel','Steel');
#6586=DESCRIPTIVE_REPRESENTATION_ITEM('Steel','Steel');
#6587=DESCRIPTIVE_REPRESENTATION_ITEM('Steel','Steel');
#6588=DESCRIPTIVE_REPRESENTATION_ITEM('Steel','Steel');
#6589=DESCRIPTIVE_REPRESENTATION_ITEM('Steel','Steel');
#6590=DESCRIPTIVE_REPRESENTATION_ITEM('Steel','Steel');
#6591=DESCRIPTIVE_REPRESENTATION_ITEM('Steel','Steel');
#6592=DESCRIPTIVE_REPRESENTATION_ITEM('Steel','Steel');
#6593=DESCRIPTIVE_REPRESENTATION_ITEM('Steel','Steel');
#6594=DESCRIPTIVE_REPRESENTATION_ITEM('Steel','Steel');
#6595=DESCRIPTIVE_REPRESENTATION_ITEM('Steel','Steel');
#6596=DESCRIPTIVE_REPRESENTATION_ITEM('Steel','Steel');
#6597=DESCRIPTIVE_REPRESENTATION_ITEM('Steel','Steel');
#6598=DESCRIPTIVE_REPRESENTATION_ITEM('Steel','Steel');
#6599=DESCRIPTIVE_REPRESENTATION_ITEM('Steel','Steel');
#6600=DESCRIPTIVE_REPRESENTATION_ITEM('Steel','Steel');
#6601=DESCRIPTIVE_REPRESENTATION_ITEM('Steel','Steel');
#6602=DESCRIPTIVE_REPRESENTATION_ITEM('Steel','Steel');
#6603=DESCRIPTIVE_REPRESENTATION_ITEM('Steel','Steel');
#6604=DESCRIPTIVE_REPRESENTATION_ITEM('Steel','Steel');
#6605=DESCRIPTIVE_REPRESENTATION_ITEM('Steel','Steel');
#6606=DESCRIPTIVE_REPRESENTATION_ITEM('Steel','Steel');
#6607=DESCRIPTIVE_REPRESENTATION_ITEM('Steel','Steel');
#6608=DESCRIPTIVE_REPRESENTATION_ITEM('Steel','Steel');
#6609=DESCRIPTIVE_REPRESENTATION_ITEM('Steel','Steel');
#6610=DESCRIPTIVE_REPRESENTATION_ITEM('Steel','Steel');
#6611=PROPERTY_DEFINITION('material property','material name',#11987);
#6612=PROPERTY_DEFINITION('material property','density of part',#11987);
#6613=PROPERTY_DEFINITION('material property','material name',#11988);
#6614=PROPERTY_DEFINITION('material property','density of part',#11988);
#6615=PROPERTY_DEFINITION('material property','material name',#11989);
#6616=PROPERTY_DEFINITION('material property','density of part',#11989);
#6617=PROPERTY_DEFINITION('material property','material name',#11990);
#6618=PROPERTY_DEFINITION('material property','density of part',#11990);
#6619=PROPERTY_DEFINITION('material property','material name',#11991);
#6620=PROPERTY_DEFINITION('material property','density of part',#11991);
#6621=PROPERTY_DEFINITION('material property','material name',#11992);
#6622=PROPERTY_DEFINITION('material property','density of part',#11992);
#6623=PROPERTY_DEFINITION('material property','material name',#11993);
#6624=PROPERTY_DEFINITION('material property','density of part',#11993);
#6625=PROPERTY_DEFINITION('material property','material name',#11994);
#6626=PROPERTY_DEFINITION('material property','density of part',#11994);
#6627=PROPERTY_DEFINITION('material property','material name',#11995);
#6628=PROPERTY_DEFINITION('material property','density of part',#11995);
#6629=PROPERTY_DEFINITION('material property','material name',#11996);
#6630=PROPERTY_DEFINITION('material property','density of part',#11996);
#6631=PROPERTY_DEFINITION('material property','material name',#11997);
#6632=PROPERTY_DEFINITION('material property','density of part',#11997);
#6633=PROPERTY_DEFINITION('material property','material name',#11998);
#6634=PROPERTY_DEFINITION('material property','density of part',#11998);
#6635=PROPERTY_DEFINITION('material property','material name',#11999);
#6636=PROPERTY_DEFINITION('material property','density of part',#11999);
#6637=PROPERTY_DEFINITION('material property','material name',#12000);
#6638=PROPERTY_DEFINITION('material property','density of part',#12000);
#6639=PROPERTY_DEFINITION('material property','material name',#12001);
#6640=PROPERTY_DEFINITION('material property','density of part',#12001);
#6641=PROPERTY_DEFINITION('material property','material name',#12003);
#6642=PROPERTY_DEFINITION('material property','density of part',#12003);
#6643=PROPERTY_DEFINITION('material property','material name',#12004);
#6644=PROPERTY_DEFINITION('material property','density of part',#12004);
#6645=PROPERTY_DEFINITION('material property','material name',#12005);
#6646=PROPERTY_DEFINITION('material property','density of part',#12005);
#6647=PROPERTY_DEFINITION('material property','material name',#12006);
#6648=PROPERTY_DEFINITION('material property','density of part',#12006);
#6649=PROPERTY_DEFINITION('material property','material name',#12007);
#6650=PROPERTY_DEFINITION('material property','density of part',#12007);
#6651=PROPERTY_DEFINITION('material property','material name',#12009);
#6652=PROPERTY_DEFINITION('material property','density of part',#12009);
#6653=PROPERTY_DEFINITION('material property','material name',#12010);
#6654=PROPERTY_DEFINITION('material property','density of part',#12010);
#6655=PROPERTY_DEFINITION('material property','material name',#12011);
#6656=PROPERTY_DEFINITION('material property','density of part',#12011);
#6657=PROPERTY_DEFINITION('material property','material name',#12012);
#6658=PROPERTY_DEFINITION('material property','density of part',#12012);
#6659=PROPERTY_DEFINITION('material property','material name',#12013);
#6660=PROPERTY_DEFINITION('material property','density of part',#12013);
#6661=PROPERTY_DEFINITION('material property','material name',#12014);
#6662=PROPERTY_DEFINITION('material property','density of part',#12014);
#6663=PROPERTY_DEFINITION('material property','material name',#12015);
#6664=PROPERTY_DEFINITION('material property','density of part',#12015);
#6665=PROPERTY_DEFINITION('material property','material name',#12016);
#6666=PROPERTY_DEFINITION('material property','density of part',#12016);
#6667=PROPERTY_DEFINITION('material property','material name',#12017);
#6668=PROPERTY_DEFINITION('material property','density of part',#12017);
#6669=PROPERTY_DEFINITION('material property','material name',#12018);
#6670=PROPERTY_DEFINITION('material property','density of part',#12018);
#6671=PROPERTY_DEFINITION('material property','material name',#12019);
#6672=PROPERTY_DEFINITION('material property','density of part',#12019);
#6673=PROPERTY_DEFINITION('material property','material name',#12020);
#6674=PROPERTY_DEFINITION('material property','density of part',#12020);
#6675=PROPERTY_DEFINITION('material property','material name',#12021);
#6676=PROPERTY_DEFINITION('material property','density of part',#12021);
#6677=PROPERTY_DEFINITION('material property','material name',#12023);
#6678=PROPERTY_DEFINITION('material property','density of part',#12023);
#6679=AXIS2_PLACEMENT_3D('',#9227,#7358,#7359);
#6680=AXIS2_PLACEMENT_3D('',#9228,#7360,#7361);
#6681=AXIS2_PLACEMENT_3D('',#9229,#7362,#7363);
#6682=AXIS2_PLACEMENT_3D('',#9230,#7364,#7365);
#6683=AXIS2_PLACEMENT_3D('',#9232,#7366,#7367);
#6684=AXIS2_PLACEMENT_3D('',#9235,#7369,#7370);
#6685=AXIS2_PLACEMENT_3D('',#9236,#7371,#7372);
#6686=AXIS2_PLACEMENT_3D('',#9238,#7373,#7374);
#6687=AXIS2_PLACEMENT_3D('',#9241,#7376,#7377);
#6688=AXIS2_PLACEMENT_3D('',#9242,#7378,#7379);
#6689=AXIS2_PLACEMENT_3D('',#9244,#7380,#7381);
#6690=AXIS2_PLACEMENT_3D('',#9247,#7383,#7384);
#6691=AXIS2_PLACEMENT_3D('',#9248,#7385,#7386);
#6692=AXIS2_PLACEMENT_3D('',#9250,#7387,#7388);
#6693=AXIS2_PLACEMENT_3D('',#9253,#7390,#7391);
#6694=AXIS2_PLACEMENT_3D('',#9254,#7392,#7393);
#6695=AXIS2_PLACEMENT_3D('',#9256,#7394,#7395);
#6696=AXIS2_PLACEMENT_3D('',#9259,#7397,#7398);
#6697=AXIS2_PLACEMENT_3D('',#9260,#7399,#7400);
#6698=AXIS2_PLACEMENT_3D('',#9262,#7401,#7402);
#6699=AXIS2_PLACEMENT_3D('',#9265,#7404,#7405);
#6700=AXIS2_PLACEMENT_3D('',#9266,#7406,#7407);
#6701=AXIS2_PLACEMENT_3D('',#9268,#7408,#7409);
#6702=AXIS2_PLACEMENT_3D('',#9271,#7411,#7412);
#6703=AXIS2_PLACEMENT_3D('',#9272,#7413,#7414);
#6704=AXIS2_PLACEMENT_3D('',#9274,#7415,#7416);
#6705=AXIS2_PLACEMENT_3D('',#9277,#7418,#7419);
#6706=AXIS2_PLACEMENT_3D('',#9278,#7420,#7421);
#6707=AXIS2_PLACEMENT_3D('',#9280,#7422,#7423);
#6708=AXIS2_PLACEMENT_3D('',#9283,#7425,#7426);
#6709=AXIS2_PLACEMENT_3D('',#9284,#7427,#7428);
#6710=AXIS2_PLACEMENT_3D('',#9286,#7429,#7430);
#6711=AXIS2_PLACEMENT_3D('',#9289,#7432,#7433);
#6712=AXIS2_PLACEMENT_3D('',#9290,#7434,#7435);
#6713=AXIS2_PLACEMENT_3D('',#9299,#7440,#7441);
#6714=AXIS2_PLACEMENT_3D('',#9305,#7445,#7446);
#6715=AXIS2_PLACEMENT_3D('',#9311,#7450,#7451);
#6716=AXIS2_PLACEMENT_3D('',#9314,#7454,#7455);
#6717=AXIS2_PLACEMENT_3D('',#9315,#7456,#7457);
#6718=AXIS2_PLACEMENT_3D('',#9316,#7458,#7459);
#6719=AXIS2_PLACEMENT_3D('',#9317,#7460,#7461);
#6720=AXIS2_PLACEMENT_3D('',#9326,#7466,#7467);
#6721=AXIS2_PLACEMENT_3D('',#9332,#7471,#7472);
#6722=AXIS2_PLACEMENT_3D('',#9338,#7476,#7477);
#6723=AXIS2_PLACEMENT_3D('',#9341,#7480,#7481);
#6724=AXIS2_PLACEMENT_3D('',#9342,#7482,#7483);
#6725=AXIS2_PLACEMENT_3D('',#9343,#7484,#7485);
#6726=AXIS2_PLACEMENT_3D('',#9344,#7486,#7487);
#6727=AXIS2_PLACEMENT_3D('',#9353,#7492,#7493);
#6728=AXIS2_PLACEMENT_3D('',#9359,#7497,#7498);
#6729=AXIS2_PLACEMENT_3D('',#9365,#7502,#7503);
#6730=AXIS2_PLACEMENT_3D('',#9368,#7506,#7507);
#6731=AXIS2_PLACEMENT_3D('',#9369,#7508,#7509);
#6732=AXIS2_PLACEMENT_3D('',#9370,#7510,#7511);
#6733=AXIS2_PLACEMENT_3D('',#9371,#7512,#7513);
#6734=AXIS2_PLACEMENT_3D('',#9373,#7514,#7515);
#6735=AXIS2_PLACEMENT_3D('',#9376,#7517,#7518);
#6736=AXIS2_PLACEMENT_3D('',#9377,#7519,#7520);
#6737=AXIS2_PLACEMENT_3D('',#9379,#7521,#7522);
#6738=AXIS2_PLACEMENT_3D('',#9380,#7523,#7524);
#6739=AXIS2_PLACEMENT_3D('',#9382,#7525,#7526);
#6740=AXIS2_PLACEMENT_3D('',#9385,#7528,#7529);
#6741=AXIS2_PLACEMENT_3D('',#9386,#7530,#7531);
#6742=AXIS2_PLACEMENT_3D('',#9388,#7532,#7533);
#6743=AXIS2_PLACEMENT_3D('',#9389,#7534,#7535);
#6744=AXIS2_PLACEMENT_3D('',#9391,#7536,#7537);
#6745=AXIS2_PLACEMENT_3D('',#9393,#7539,#7540);
#6746=AXIS2_PLACEMENT_3D('',#9395,#7541,#7542);
#6747=AXIS2_PLACEMENT_3D('',#9397,#7544,#7545);
#6748=AXIS2_PLACEMENT_3D('',#9399,#7546,#7547);
#6749=AXIS2_PLACEMENT_3D('',#9402,#7549,#7550);
#6750=AXIS2_PLACEMENT_3D('',#9403,#7551,#7552);
#6751=AXIS2_PLACEMENT_3D('',#9405,#7553,#7554);
#6752=AXIS2_PLACEMENT_3D('',#9406,#7555,#7556);
#6753=AXIS2_PLACEMENT_3D('',#9408,#7557,#7558);
#6754=AXIS2_PLACEMENT_3D('',#9411,#7560,#7561);
#6755=AXIS2_PLACEMENT_3D('',#9412,#7562,#7563);
#6756=AXIS2_PLACEMENT_3D('',#9414,#7564,#7565);
#6757=AXIS2_PLACEMENT_3D('',#9415,#7566,#7567);
#6758=AXIS2_PLACEMENT_3D('',#9417,#7568,#7569);
#6759=AXIS2_PLACEMENT_3D('',#9419,#7571,#7572);
#6760=AXIS2_PLACEMENT_3D('',#9421,#7573,#7574);
#6761=AXIS2_PLACEMENT_3D('',#9423,#7576,#7577);
#6762=AXIS2_PLACEMENT_3D('',#9425,#7578,#7579);
#6763=AXIS2_PLACEMENT_3D('',#9428,#7581,#7582);
#6764=AXIS2_PLACEMENT_3D('',#9429,#7583,#7584);
#6765=AXIS2_PLACEMENT_3D('',#9431,#7585,#7586);
#6766=AXIS2_PLACEMENT_3D('',#9434,#7588,#7589);
#6767=AXIS2_PLACEMENT_3D('',#9435,#7590,#7591);
#6768=AXIS2_PLACEMENT_3D('',#9444,#7596,#7597);
#6769=AXIS2_PLACEMENT_3D('',#9450,#7601,#7602);
#6770=AXIS2_PLACEMENT_3D('',#9456,#7606,#7607);
#6771=AXIS2_PLACEMENT_3D('',#9459,#7610,#7611);
#6772=AXIS2_PLACEMENT_3D('',#9460,#7612,#7613);
#6773=AXIS2_PLACEMENT_3D('',#9461,#7614,#7615);
#6774=AXIS2_PLACEMENT_3D('',#9462,#7616,#7617);
#6775=AXIS2_PLACEMENT_3D('',#9464,#7618,#7619);
#6776=AXIS2_PLACEMENT_3D('',#9467,#7621,#7622);
#6777=AXIS2_PLACEMENT_3D('',#9468,#7623,#7624);
#6778=AXIS2_PLACEMENT_3D('',#9470,#7625,#7626);
#6779=AXIS2_PLACEMENT_3D('',#9473,#7628,#7629);
#6780=AXIS2_PLACEMENT_3D('',#9474,#7630,#7631);
#6781=AXIS2_PLACEMENT_3D('',#9475,#7632,#7633);
#6782=AXIS2_PLACEMENT_3D('',#9476,#7634,#7635);
#6783=AXIS2_PLACEMENT_3D('',#9477,#7636,#7637);
#6784=AXIS2_PLACEMENT_3D('',#9479,#7638,#7639);
#6785=AXIS2_PLACEMENT_3D('',#9482,#7641,#7642);
#6786=AXIS2_PLACEMENT_3D('',#9483,#7643,#7644);
#6787=AXIS2_PLACEMENT_3D('',#9485,#7645,#7646);
#6788=AXIS2_PLACEMENT_3D('',#9488,#7648,#7649);
#6789=AXIS2_PLACEMENT_3D('',#9489,#7650,#7651);
#6790=AXIS2_PLACEMENT_3D('',#9490,#7652,#7653);
#6791=AXIS2_PLACEMENT_3D('',#9491,#7654,#7655);
#6792=AXIS2_PLACEMENT_3D('',#9492,#7656,#7657);
#6793=AXIS2_PLACEMENT_3D('',#9494,#7658,#7659);
#6794=AXIS2_PLACEMENT_3D('',#9497,#7661,#7662);
#6795=AXIS2_PLACEMENT_3D('',#9498,#7663,#7664);
#6796=AXIS2_PLACEMENT_3D('',#9500,#7665,#7666);
#6797=AXIS2_PLACEMENT_3D('',#9501,#7667,#7668);
#6798=AXIS2_PLACEMENT_3D('',#9503,#7669,#7670);
#6799=AXIS2_PLACEMENT_3D('',#9506,#7672,#7673);
#6800=AXIS2_PLACEMENT_3D('',#9507,#7674,#7675);
#6801=AXIS2_PLACEMENT_3D('',#9509,#7676,#7677);
#6802=AXIS2_PLACEMENT_3D('',#9510,#7678,#7679);
#6803=AXIS2_PLACEMENT_3D('',#9512,#7680,#7681);
#6804=AXIS2_PLACEMENT_3D('',#9514,#7683,#7684);
#6805=AXIS2_PLACEMENT_3D('',#9516,#7685,#7686);
#6806=AXIS2_PLACEMENT_3D('',#9518,#7688,#7689);
#6807=AXIS2_PLACEMENT_3D('',#9520,#7690,#7691);
#6808=AXIS2_PLACEMENT_3D('',#9523,#7693,#7694);
#6809=AXIS2_PLACEMENT_3D('',#9524,#7695,#7696);
#6810=AXIS2_PLACEMENT_3D('',#9526,#7697,#7698);
#6811=AXIS2_PLACEMENT_3D('',#9527,#7699,#7700);
#6812=AXIS2_PLACEMENT_3D('',#9529,#7701,#7702);
#6813=AXIS2_PLACEMENT_3D('',#9532,#7704,#7705);
#6814=AXIS2_PLACEMENT_3D('',#9533,#7706,#7707);
#6815=AXIS2_PLACEMENT_3D('',#9535,#7708,#7709);
#6816=AXIS2_PLACEMENT_3D('',#9536,#7710,#7711);
#6817=AXIS2_PLACEMENT_3D('',#9538,#7712,#7713);
#6818=AXIS2_PLACEMENT_3D('',#9540,#7715,#7716);
#6819=AXIS2_PLACEMENT_3D('',#9542,#7717,#7718);
#6820=AXIS2_PLACEMENT_3D('',#9544,#7720,#7721);
#6821=AXIS2_PLACEMENT_3D('',#9546,#7722,#7723);
#6822=AXIS2_PLACEMENT_3D('',#9549,#7725,#7726);
#6823=AXIS2_PLACEMENT_3D('',#9550,#7727,#7728);
#6824=AXIS2_PLACEMENT_3D('',#9552,#7729,#7730);
#6825=AXIS2_PLACEMENT_3D('',#9555,#7732,#7733);
#6826=AXIS2_PLACEMENT_3D('',#9556,#7734,#7735);
#6827=AXIS2_PLACEMENT_3D('',#9565,#7740,#7741);
#6828=AXIS2_PLACEMENT_3D('',#9571,#7745,#7746);
#6829=AXIS2_PLACEMENT_3D('',#9577,#7750,#7751);
#6830=AXIS2_PLACEMENT_3D('',#9580,#7754,#7755);
#6831=AXIS2_PLACEMENT_3D('',#9581,#7756,#7757);
#6832=AXIS2_PLACEMENT_3D('',#9582,#7758,#7759);
#6833=AXIS2_PLACEMENT_3D('',#9583,#7760,#7761);
#6834=AXIS2_PLACEMENT_3D('',#9585,#7762,#7763);
#6835=AXIS2_PLACEMENT_3D('',#9588,#7765,#7766);
#6836=AXIS2_PLACEMENT_3D('',#9589,#7767,#7768);
#6837=AXIS2_PLACEMENT_3D('',#9591,#7769,#7770);
#6838=AXIS2_PLACEMENT_3D('',#9594,#7772,#7773);
#6839=AXIS2_PLACEMENT_3D('',#9595,#7774,#7775);
#6840=AXIS2_PLACEMENT_3D('',#9596,#7776,#7777);
#6841=AXIS2_PLACEMENT_3D('',#9597,#7778,#7779);
#6842=AXIS2_PLACEMENT_3D('',#9598,#7780,#7781);
#6843=AXIS2_PLACEMENT_3D('',#9600,#7782,#7783);
#6844=AXIS2_PLACEMENT_3D('',#9603,#7785,#7786);
#6845=AXIS2_PLACEMENT_3D('',#9604,#7787,#7788);
#6846=AXIS2_PLACEMENT_3D('',#9606,#7789,#7790);
#6847=AXIS2_PLACEMENT_3D('',#9609,#7792,#7793);
#6848=AXIS2_PLACEMENT_3D('',#9610,#7794,#7795);
#6849=AXIS2_PLACEMENT_3D('',#9611,#7796,#7797);
#6850=AXIS2_PLACEMENT_3D('',#9612,#7798,#7799);
#6851=AXIS2_PLACEMENT_3D('',#9613,#7800,#7801);
#6852=AXIS2_PLACEMENT_3D('',#9615,#7802,#7803);
#6853=AXIS2_PLACEMENT_3D('',#9618,#7805,#7806);
#6854=AXIS2_PLACEMENT_3D('',#9619,#7807,#7808);
#6855=AXIS2_PLACEMENT_3D('',#9621,#7809,#7810);
#6856=AXIS2_PLACEMENT_3D('',#9624,#7812,#7813);
#6857=AXIS2_PLACEMENT_3D('',#9625,#7814,#7815);
#6858=AXIS2_PLACEMENT_3D('',#9627,#7816,#7817);
#6859=AXIS2_PLACEMENT_3D('',#9630,#7819,#7820);
#6860=AXIS2_PLACEMENT_3D('',#9631,#7821,#7822);
#6861=AXIS2_PLACEMENT_3D('',#9648,#7831,#7832);
#6862=AXIS2_PLACEMENT_3D('',#9654,#7836,#7837);
#6863=AXIS2_PLACEMENT_3D('',#9660,#7841,#7842);
#6864=AXIS2_PLACEMENT_3D('',#9662,#7844,#7845);
#6865=AXIS2_PLACEMENT_3D('',#9664,#7847,#7848);
#6866=AXIS2_PLACEMENT_3D('',#9670,#7852,#7853);
#6867=AXIS2_PLACEMENT_3D('',#9674,#7856,#7857);
#6868=AXIS2_PLACEMENT_3D('',#9678,#7860,#7861);
#6869=AXIS2_PLACEMENT_3D('',#9680,#7863,#7864);
#6870=AXIS2_PLACEMENT_3D('',#9681,#7865,#7866);
#6871=AXIS2_PLACEMENT_3D('',#9682,#7867,#7868);
#6872=AXIS2_PLACEMENT_3D('',#9683,#7869,#7870);
#6873=AXIS2_PLACEMENT_3D('',#9685,#7871,#7872);
#6874=AXIS2_PLACEMENT_3D('',#9688,#7874,#7875);
#6875=AXIS2_PLACEMENT_3D('',#9689,#7876,#7877);
#6876=AXIS2_PLACEMENT_3D('',#9690,#7878,#7879);
#6877=AXIS2_PLACEMENT_3D('',#9692,#7880,#7881);
#6878=AXIS2_PLACEMENT_3D('',#9694,#7882,#7883);
#6879=AXIS2_PLACEMENT_3D('',#9695,#7884,#7885);
#6880=AXIS2_PLACEMENT_3D('',#9698,#7887,#7888);
#6881=AXIS2_PLACEMENT_3D('',#9699,#7889,#7890);
#6882=AXIS2_PLACEMENT_3D('',#9700,#7891,#7892);
#6883=AXIS2_PLACEMENT_3D('',#9702,#7893,#7894);
#6884=AXIS2_PLACEMENT_3D('',#9704,#7896,#7897);
#6885=AXIS2_PLACEMENT_3D('',#9705,#7898,#7899);
#6886=AXIS2_PLACEMENT_3D('',#9706,#7900,#7901);
#6887=AXIS2_PLACEMENT_3D('',#9708,#7902,#7903);
#6888=AXIS2_PLACEMENT_3D('',#9711,#7905,#7906);
#6889=AXIS2_PLACEMENT_3D('',#9712,#7907,#7908);
#6890=AXIS2_PLACEMENT_3D('',#9714,#7909,#7910);
#6891=AXIS2_PLACEMENT_3D('',#9717,#7912,#7913);
#6892=AXIS2_PLACEMENT_3D('',#9718,#7914,#7915);
#6893=AXIS2_PLACEMENT_3D('',#9719,#7916,#7917);
#6894=AXIS2_PLACEMENT_3D('',#9720,#7918,#7919);
#6895=AXIS2_PLACEMENT_3D('',#9721,#7920,#7921);
#6896=AXIS2_PLACEMENT_3D('',#9723,#7922,#7923);
#6897=AXIS2_PLACEMENT_3D('',#9726,#7925,#7926);
#6898=AXIS2_PLACEMENT_3D('',#9727,#7927,#7928);
#6899=AXIS2_PLACEMENT_3D('',#9729,#7929,#7930);
#6900=AXIS2_PLACEMENT_3D('',#9732,#7932,#7933);
#6901=AXIS2_PLACEMENT_3D('',#9733,#7934,#7935);
#6902=AXIS2_PLACEMENT_3D('',#9734,#7936,#7937);
#6903=AXIS2_PLACEMENT_3D('',#9735,#7938,#7939);
#6904=AXIS2_PLACEMENT_3D('',#9736,#7940,#7941);
#6905=AXIS2_PLACEMENT_3D('',#9745,#7946,#7947);
#6906=AXIS2_PLACEMENT_3D('',#9751,#7951,#7952);
#6907=AXIS2_PLACEMENT_3D('',#9757,#7956,#7957);
#6908=AXIS2_PLACEMENT_3D('',#9760,#7960,#7961);
#6909=AXIS2_PLACEMENT_3D('',#9761,#7962,#7963);
#6910=AXIS2_PLACEMENT_3D('',#9762,#7964,#7965);
#6911=AXIS2_PLACEMENT_3D('',#9763,#7966,#7967);
#6912=AXIS2_PLACEMENT_3D('',#9765,#7968,#7969);
#6913=AXIS2_PLACEMENT_3D('',#9768,#7971,#7972);
#6914=AXIS2_PLACEMENT_3D('',#9769,#7973,#7974);
#6915=AXIS2_PLACEMENT_3D('',#9778,#7979,#7980);
#6916=AXIS2_PLACEMENT_3D('',#9784,#7984,#7985);
#6917=AXIS2_PLACEMENT_3D('',#9790,#7989,#7990);
#6918=AXIS2_PLACEMENT_3D('',#9793,#7993,#7994);
#6919=AXIS2_PLACEMENT_3D('',#9794,#7995,#7996);
#6920=AXIS2_PLACEMENT_3D('',#9795,#7997,#7998);
#6921=AXIS2_PLACEMENT_3D('',#9796,#7999,#8000);
#6922=AXIS2_PLACEMENT_3D('',#9797,#8001,#8002);
#6923=AXIS2_PLACEMENT_3D('',#9799,#8003,#8004);
#6924=AXIS2_PLACEMENT_3D('',#9802,#8006,#8007);
#6925=AXIS2_PLACEMENT_3D('',#9803,#8008,#8009);
#6926=AXIS2_PLACEMENT_3D('',#9805,#8010,#8011);
#6927=AXIS2_PLACEMENT_3D('',#9808,#8013,#8014);
#6928=AXIS2_PLACEMENT_3D('',#9809,#8015,#8016);
#6929=AXIS2_PLACEMENT_3D('',#9812,#8017,#8018);
#6930=AXIS2_PLACEMENT_3D('',#9813,#8019,#8020);
#6931=AXIS2_PLACEMENT_3D('',#9819,#8023,#8024);
#6932=AXIS2_PLACEMENT_3D('',#9820,#8025,#8026);
#6933=AXIS2_PLACEMENT_3D('',#9825,#8028,#8029);
#6934=AXIS2_PLACEMENT_3D('',#9827,#8031,#8032);
#6935=AXIS2_PLACEMENT_3D('',#9832,#8034,#8035);
#6936=AXIS2_PLACEMENT_3D('',#9834,#8037,#8038);
#6937=AXIS2_PLACEMENT_3D('',#9837,#8041,#8042);
#6938=AXIS2_PLACEMENT_3D('',#9843,#8045,#8046);
#6939=AXIS2_PLACEMENT_3D('',#9844,#8047,#8048);
#6940=AXIS2_PLACEMENT_3D('',#9847,#8051,#8052);
#6941=AXIS2_PLACEMENT_3D('',#9857,#8057,#8058);
#6942=AXIS2_PLACEMENT_3D('',#9859,#8059,#8060);
#6943=AXIS2_PLACEMENT_3D('',#9870,#8067,#8068);
#6944=AXIS2_PLACEMENT_3D('',#9871,#8069,#8070);
#6945=AXIS2_PLACEMENT_3D('',#9872,#8071,#8072);
#6946=AXIS2_PLACEMENT_3D('',#9873,#8073,#8074);
#6947=AXIS2_PLACEMENT_3D('',#9874,#8075,#8076);
#6948=AXIS2_PLACEMENT_3D('',#9875,#8077,#8078);
#6949=AXIS2_PLACEMENT_3D('',#9884,#8083,#8084);
#6950=AXIS2_PLACEMENT_3D('',#9890,#8088,#8089);
#6951=AXIS2_PLACEMENT_3D('',#9896,#8093,#8094);
#6952=AXIS2_PLACEMENT_3D('',#9899,#8097,#8098);
#6953=AXIS2_PLACEMENT_3D('',#9900,#8099,#8100);
#6954=AXIS2_PLACEMENT_3D('',#9902,#8101,#8102);
#6955=AXIS2_PLACEMENT_3D('',#9904,#8104,#8105);
#6956=AXIS2_PLACEMENT_3D('',#9906,#8106,#8107);
#6957=AXIS2_PLACEMENT_3D('',#9908,#8109,#8110);
#6958=AXIS2_PLACEMENT_3D('',#9914,#8114,#8115);
#6959=AXIS2_PLACEMENT_3D('',#9918,#8118,#8119);
#6960=AXIS2_PLACEMENT_3D('',#9922,#8122,#8123);
#6961=AXIS2_PLACEMENT_3D('',#9924,#8125,#8126);
#6962=AXIS2_PLACEMENT_3D('',#9925,#8127,#8128);
#6963=AXIS2_PLACEMENT_3D('',#9926,#8129,#8130);
#6964=AXIS2_PLACEMENT_3D('',#9928,#8131,#8132);
#6965=AXIS2_PLACEMENT_3D('',#9931,#8134,#8135);
#6966=AXIS2_PLACEMENT_3D('',#9932,#8136,#8137);
#6967=AXIS2_PLACEMENT_3D('',#9934,#8138,#8139);
#6968=AXIS2_PLACEMENT_3D('',#9935,#8140,#8141);
#6969=AXIS2_PLACEMENT_3D('',#9938,#8142,#8143);
#6970=AXIS2_PLACEMENT_3D('',#9940,#8144,#8145);
#6971=AXIS2_PLACEMENT_3D('',#9941,#8146,#8147);
#6972=AXIS2_PLACEMENT_3D('',#9942,#8148,#8149);
#6973=AXIS2_PLACEMENT_3D('',#10020,#8151,#8152);
#6974=AXIS2_PLACEMENT_3D('',#10098,#8154,#8155);
#6975=AXIS2_PLACEMENT_3D('',#10100,#8156,#8157);
#6976=AXIS2_PLACEMENT_3D('',#10103,#8159,#8160);
#6977=AXIS2_PLACEMENT_3D('',#10268,#8161,#8162);
#6978=AXIS2_PLACEMENT_3D('',#10305,#8164,#8165);
#6979=AXIS2_PLACEMENT_3D('',#10342,#8167,#8168);
#6980=AXIS2_PLACEMENT_3D('',#10379,#8170,#8171);
#6981=AXIS2_PLACEMENT_3D('',#10416,#8173,#8174);
#6982=AXIS2_PLACEMENT_3D('',#10418,#8175,#8176);
#6983=AXIS2_PLACEMENT_3D('',#10419,#8177,#8178);
#6984=AXIS2_PLACEMENT_3D('',#10421,#8179,#8180);
#6985=AXIS2_PLACEMENT_3D('',#10422,#8181,#8182);
#6986=AXIS2_PLACEMENT_3D('',#10424,#8183,#8184);
#6987=AXIS2_PLACEMENT_3D('',#10426,#8186,#8187);
#6988=AXIS2_PLACEMENT_3D('',#10428,#8188,#8189);
#6989=AXIS2_PLACEMENT_3D('',#10429,#8190,#8191);
#6990=AXIS2_PLACEMENT_3D('',#10431,#8193,#8194);
#6991=AXIS2_PLACEMENT_3D('',#10432,#8195,#8196);
#6992=AXIS2_PLACEMENT_3D('',#10433,#8197,#8198);
#6993=AXIS2_PLACEMENT_3D('',#10434,#8199,#8200);
#6994=AXIS2_PLACEMENT_3D('',#10436,#8201,#8202);
#6995=AXIS2_PLACEMENT_3D('',#10439,#8204,#8205);
#6996=AXIS2_PLACEMENT_3D('',#10440,#8206,#8207);
#6997=AXIS2_PLACEMENT_3D('',#10442,#8208,#8209);
#6998=AXIS2_PLACEMENT_3D('',#10445,#8211,#8212);
#6999=AXIS2_PLACEMENT_3D('',#10446,#8213,#8214);
#7000=AXIS2_PLACEMENT_3D('',#10447,#8215,#8216);
#7001=AXIS2_PLACEMENT_3D('',#10448,#8217,#8218);
#7002=AXIS2_PLACEMENT_3D('',#10449,#8219,#8220);
#7003=AXIS2_PLACEMENT_3D('',#10458,#8225,#8226);
#7004=AXIS2_PLACEMENT_3D('',#10464,#8230,#8231);
#7005=AXIS2_PLACEMENT_3D('',#10470,#8235,#8236);
#7006=AXIS2_PLACEMENT_3D('',#10476,#8240,#8241);
#7007=AXIS2_PLACEMENT_3D('',#10482,#8245,#8246);
#7008=AXIS2_PLACEMENT_3D('',#10485,#8249,#8250);
#7009=AXIS2_PLACEMENT_3D('',#10486,#8251,#8252);
#7010=AXIS2_PLACEMENT_3D('',#10487,#8253,#8254);
#7011=AXIS2_PLACEMENT_3D('',#10489,#8255,#8256);
#7012=AXIS2_PLACEMENT_3D('',#10490,#8257,#8258);
#7013=AXIS2_PLACEMENT_3D('',#10492,#8259,#8260);
#7014=AXIS2_PLACEMENT_3D('',#10493,#8261,#8262);
#7015=AXIS2_PLACEMENT_3D('',#10495,#8263,#8264);
#7016=AXIS2_PLACEMENT_3D('',#10497,#8266,#8267);
#7017=AXIS2_PLACEMENT_3D('',#10499,#8268,#8269);
#7018=AXIS2_PLACEMENT_3D('',#10501,#8271,#8272);
#7019=AXIS2_PLACEMENT_3D('',#10503,#8273,#8274);
#7020=AXIS2_PLACEMENT_3D('',#10505,#8276,#8277);
#7021=AXIS2_PLACEMENT_3D('',#10507,#8278,#8279);
#7022=AXIS2_PLACEMENT_3D('',#10508,#8280,#8281);
#7023=AXIS2_PLACEMENT_3D('',#10510,#8282,#8283);
#7024=AXIS2_PLACEMENT_3D('',#10512,#8285,#8286);
#7025=AXIS2_PLACEMENT_3D('',#10514,#8288,#8289);
#7026=AXIS2_PLACEMENT_3D('',#10515,#8290,#8291);
#7027=AXIS2_PLACEMENT_3D('',#10524,#8296,#8297);
#7028=AXIS2_PLACEMENT_3D('',#10530,#8301,#8302);
#7029=AXIS2_PLACEMENT_3D('',#10536,#8306,#8307);
#7030=AXIS2_PLACEMENT_3D('',#10542,#8311,#8312);
#7031=AXIS2_PLACEMENT_3D('',#10548,#8316,#8317);
#7032=AXIS2_PLACEMENT_3D('',#10551,#8320,#8321);
#7033=AXIS2_PLACEMENT_3D('',#10552,#8322,#8323);
#7034=AXIS2_PLACEMENT_3D('',#10553,#8324,#8325);
#7035=AXIS2_PLACEMENT_3D('',#10555,#8326,#8327);
#7036=AXIS2_PLACEMENT_3D('',#10556,#8328,#8329);
#7037=AXIS2_PLACEMENT_3D('',#10558,#8330,#8331);
#7038=AXIS2_PLACEMENT_3D('',#10559,#8332,#8333);
#7039=AXIS2_PLACEMENT_3D('',#10561,#8334,#8335);
#7040=AXIS2_PLACEMENT_3D('',#10563,#8337,#8338);
#7041=AXIS2_PLACEMENT_3D('',#10565,#8339,#8340);
#7042=AXIS2_PLACEMENT_3D('',#10567,#8342,#8343);
#7043=AXIS2_PLACEMENT_3D('',#10569,#8344,#8345);
#7044=AXIS2_PLACEMENT_3D('',#10571,#8347,#8348);
#7045=AXIS2_PLACEMENT_3D('',#10573,#8349,#8350);
#7046=AXIS2_PLACEMENT_3D('',#10574,#8351,#8352);
#7047=AXIS2_PLACEMENT_3D('',#10576,#8353,#8354);
#7048=AXIS2_PLACEMENT_3D('',#10578,#8356,#8357);
#7049=AXIS2_PLACEMENT_3D('',#10580,#8359,#8360);
#7050=AXIS2_PLACEMENT_3D('',#10581,#8361,#8362);
#7051=AXIS2_PLACEMENT_3D('',#10582,#8363,#8364);
#7052=AXIS2_PLACEMENT_3D('',#10584,#8365,#8366);
#7053=AXIS2_PLACEMENT_3D('',#10587,#8368,#8369);
#7054=AXIS2_PLACEMENT_3D('',#10588,#8370,#8371);
#7055=AXIS2_PLACEMENT_3D('',#10589,#8372,#8373);
#7056=AXIS2_PLACEMENT_3D('',#10590,#8374,#8375);
#7057=AXIS2_PLACEMENT_3D('',#10591,#8376,#8377);
#7058=AXIS2_PLACEMENT_3D('',#10595,#8379,#8380);
#7059=AXIS2_PLACEMENT_3D('',#10596,#8381,#8382);
#7060=AXIS2_PLACEMENT_3D('',#10613,#8383,#8384);
#7061=AXIS2_PLACEMENT_3D('',#10654,#8386,#8387);
#7062=AXIS2_PLACEMENT_3D('',#10669,#8388,#8389);
#7063=AXIS2_PLACEMENT_3D('',#10671,#8391,#8392);
#7064=AXIS2_PLACEMENT_3D('',#10673,#8393,#8394);
#7065=AXIS2_PLACEMENT_3D('',#10676,#8396,#8397);
#7066=AXIS2_PLACEMENT_3D('',#10677,#8398,#8399);
#7067=AXIS2_PLACEMENT_3D('',#10679,#8400,#8401);
#7068=AXIS2_PLACEMENT_3D('',#10682,#8403,#8404);
#7069=AXIS2_PLACEMENT_3D('',#10683,#8405,#8406);
#7070=AXIS2_PLACEMENT_3D('',#10684,#8407,#8408);
#7071=AXIS2_PLACEMENT_3D('',#10685,#8409,#8410);
#7072=AXIS2_PLACEMENT_3D('',#10686,#8411,#8412);
#7073=AXIS2_PLACEMENT_3D('',#10690,#8414,#8415);
#7074=AXIS2_PLACEMENT_3D('',#10691,#8416,#8417);
#7075=AXIS2_PLACEMENT_3D('',#10708,#8418,#8419);
#7076=AXIS2_PLACEMENT_3D('',#10749,#8421,#8422);
#7077=AXIS2_PLACEMENT_3D('',#10764,#8423,#8424);
#7078=AXIS2_PLACEMENT_3D('',#10766,#8426,#8427);
#7079=AXIS2_PLACEMENT_3D('',#10768,#8428,#8429);
#7080=AXIS2_PLACEMENT_3D('',#10771,#8431,#8432);
#7081=AXIS2_PLACEMENT_3D('',#10772,#8433,#8434);
#7082=AXIS2_PLACEMENT_3D('',#10774,#8435,#8436);
#7083=AXIS2_PLACEMENT_3D('',#10777,#8438,#8439);
#7084=AXIS2_PLACEMENT_3D('',#10778,#8440,#8441);
#7085=AXIS2_PLACEMENT_3D('',#10779,#8442,#8443);
#7086=AXIS2_PLACEMENT_3D('',#10780,#8444,#8445);
#7087=AXIS2_PLACEMENT_3D('',#10781,#8446,#8447);
#7088=AXIS2_PLACEMENT_3D('',#10783,#8448,#8449);
#7089=AXIS2_PLACEMENT_3D('',#10786,#8451,#8452);
#7090=AXIS2_PLACEMENT_3D('',#10787,#8453,#8454);
#7091=AXIS2_PLACEMENT_3D('',#10789,#8455,#8456);
#7092=AXIS2_PLACEMENT_3D('',#10792,#8458,#8459);
#7093=AXIS2_PLACEMENT_3D('',#10793,#8460,#8461);
#7094=AXIS2_PLACEMENT_3D('',#10794,#8462,#8463);
#7095=AXIS2_PLACEMENT_3D('',#10795,#8464,#8465);
#7096=AXIS2_PLACEMENT_3D('',#10796,#8466,#8467);
#7097=AXIS2_PLACEMENT_3D('',#10798,#8468,#8469);
#7098=AXIS2_PLACEMENT_3D('',#10801,#8471,#8472);
#7099=AXIS2_PLACEMENT_3D('',#10802,#8473,#8474);
#7100=AXIS2_PLACEMENT_3D('',#10804,#8475,#8476);
#7101=AXIS2_PLACEMENT_3D('',#10807,#8478,#8479);
#7102=AXIS2_PLACEMENT_3D('',#10808,#8480,#8481);
#7103=AXIS2_PLACEMENT_3D('',#10809,#8482,#8483);
#7104=AXIS2_PLACEMENT_3D('',#10810,#8484,#8485);
#7105=AXIS2_PLACEMENT_3D('',#10811,#8486,#8487);
#7106=AXIS2_PLACEMENT_3D('',#10815,#8489,#8490);
#7107=AXIS2_PLACEMENT_3D('',#10816,#8491,#8492);
#7108=AXIS2_PLACEMENT_3D('',#10833,#8493,#8494);
#7109=AXIS2_PLACEMENT_3D('',#10874,#8496,#8497);
#7110=AXIS2_PLACEMENT_3D('',#10889,#8498,#8499);
#7111=AXIS2_PLACEMENT_3D('',#10891,#8501,#8502);
#7112=AXIS2_PLACEMENT_3D('',#10893,#8503,#8504);
#7113=AXIS2_PLACEMENT_3D('',#10896,#8506,#8507);
#7114=AXIS2_PLACEMENT_3D('',#10897,#8508,#8509);
#7115=AXIS2_PLACEMENT_3D('',#10899,#8510,#8511);
#7116=AXIS2_PLACEMENT_3D('',#10902,#8513,#8514);
#7117=AXIS2_PLACEMENT_3D('',#10903,#8515,#8516);
#7118=AXIS2_PLACEMENT_3D('',#10904,#8517,#8518);
#7119=AXIS2_PLACEMENT_3D('',#10905,#8519,#8520);
#7120=AXIS2_PLACEMENT_3D('',#10906,#8521,#8522);
#7121=AXIS2_PLACEMENT_3D('',#10908,#8523,#8524);
#7122=AXIS2_PLACEMENT_3D('',#10911,#8526,#8527);
#7123=AXIS2_PLACEMENT_3D('',#10912,#8528,#8529);
#7124=AXIS2_PLACEMENT_3D('',#10914,#8530,#8531);
#7125=AXIS2_PLACEMENT_3D('',#10917,#8533,#8534);
#7126=AXIS2_PLACEMENT_3D('',#10918,#8535,#8536);
#7127=AXIS2_PLACEMENT_3D('',#10919,#8537,#8538);
#7128=AXIS2_PLACEMENT_3D('',#10920,#8539,#8540);
#7129=AXIS2_PLACEMENT_3D('',#10921,#8541,#8542);
#7130=AXIS2_PLACEMENT_3D('',#10925,#8544,#8545);
#7131=AXIS2_PLACEMENT_3D('',#10926,#8546,#8547);
#7132=AXIS2_PLACEMENT_3D('',#10943,#8548,#8549);
#7133=AXIS2_PLACEMENT_3D('',#10984,#8551,#8552);
#7134=AXIS2_PLACEMENT_3D('',#10999,#8553,#8554);
#7135=AXIS2_PLACEMENT_3D('',#11001,#8556,#8557);
#7136=AXIS2_PLACEMENT_3D('',#11003,#8558,#8559);
#7137=AXIS2_PLACEMENT_3D('',#11006,#8561,#8562);
#7138=AXIS2_PLACEMENT_3D('',#11007,#8563,#8564);
#7139=AXIS2_PLACEMENT_3D('',#11009,#8565,#8566);
#7140=AXIS2_PLACEMENT_3D('',#11012,#8568,#8569);
#7141=AXIS2_PLACEMENT_3D('',#11013,#8570,#8571);
#7142=AXIS2_PLACEMENT_3D('',#11014,#8572,#8573);
#7143=AXIS2_PLACEMENT_3D('',#11015,#8574,#8575);
#7144=AXIS2_PLACEMENT_3D('',#11016,#8576,#8577);
#7145=AXIS2_PLACEMENT_3D('',#11020,#8579,#8580);
#7146=AXIS2_PLACEMENT_3D('',#11021,#8581,#8582);
#7147=AXIS2_PLACEMENT_3D('',#11038,#8583,#8584);
#7148=AXIS2_PLACEMENT_3D('',#11079,#8586,#8587);
#7149=AXIS2_PLACEMENT_3D('',#11094,#8588,#8589);
#7150=AXIS2_PLACEMENT_3D('',#11096,#8591,#8592);
#7151=AXIS2_PLACEMENT_3D('',#11098,#8593,#8594);
#7152=AXIS2_PLACEMENT_3D('',#11101,#8596,#8597);
#7153=AXIS2_PLACEMENT_3D('',#11102,#8598,#8599);
#7154=AXIS2_PLACEMENT_3D('',#11104,#8600,#8601);
#7155=AXIS2_PLACEMENT_3D('',#11105,#8602,#8603);
#7156=AXIS2_PLACEMENT_3D('',#11107,#8604,#8605);
#7157=AXIS2_PLACEMENT_3D('',#11109,#8607,#8608);
#7158=AXIS2_PLACEMENT_3D('',#11118,#8613,#8614);
#7159=AXIS2_PLACEMENT_3D('',#11124,#8618,#8619);
#7160=AXIS2_PLACEMENT_3D('',#11130,#8623,#8624);
#7161=AXIS2_PLACEMENT_3D('',#11136,#8628,#8629);
#7162=AXIS2_PLACEMENT_3D('',#11142,#8633,#8634);
#7163=AXIS2_PLACEMENT_3D('',#11148,#8638,#8639);
#7164=AXIS2_PLACEMENT_3D('',#11154,#8643,#8644);
#7165=AXIS2_PLACEMENT_3D('',#11160,#8648,#8649);
#7166=AXIS2_PLACEMENT_3D('',#11166,#8653,#8654);
#7167=AXIS2_PLACEMENT_3D('',#11172,#8658,#8659);
#7168=AXIS2_PLACEMENT_3D('',#11178,#8663,#8664);
#7169=AXIS2_PLACEMENT_3D('',#11184,#8668,#8669);
#7170=AXIS2_PLACEMENT_3D('',#11190,#8673,#8674);
#7171=AXIS2_PLACEMENT_3D('',#11196,#8678,#8679);
#7172=AXIS2_PLACEMENT_3D('',#11202,#8683,#8684);
#7173=AXIS2_PLACEMENT_3D('',#11208,#8688,#8689);
#7174=AXIS2_PLACEMENT_3D('',#11214,#8693,#8694);
#7175=AXIS2_PLACEMENT_3D('',#11220,#8698,#8699);
#7176=AXIS2_PLACEMENT_3D('',#11226,#8703,#8704);
#7177=AXIS2_PLACEMENT_3D('',#11232,#8708,#8709);
#7178=AXIS2_PLACEMENT_3D('',#11238,#8713,#8714);
#7179=AXIS2_PLACEMENT_3D('',#11244,#8718,#8719);
#7180=AXIS2_PLACEMENT_3D('',#11250,#8723,#8724);
#7181=AXIS2_PLACEMENT_3D('',#11256,#8728,#8729);
#7182=AXIS2_PLACEMENT_3D('',#11262,#8733,#8734);
#7183=AXIS2_PLACEMENT_3D('',#11268,#8738,#8739);
#7184=AXIS2_PLACEMENT_3D('',#11274,#8743,#8744);
#7185=AXIS2_PLACEMENT_3D('',#11280,#8748,#8749);
#7186=AXIS2_PLACEMENT_3D('',#11286,#8753,#8754);
#7187=AXIS2_PLACEMENT_3D('',#11292,#8758,#8759);
#7188=AXIS2_PLACEMENT_3D('',#11298,#8763,#8764);
#7189=AXIS2_PLACEMENT_3D('',#11304,#8768,#8769);
#7190=AXIS2_PLACEMENT_3D('',#11310,#8773,#8774);
#7191=AXIS2_PLACEMENT_3D('',#11316,#8778,#8779);
#7192=AXIS2_PLACEMENT_3D('',#11322,#8783,#8784);
#7193=AXIS2_PLACEMENT_3D('',#11328,#8788,#8789);
#7194=AXIS2_PLACEMENT_3D('',#11334,#8793,#8794);
#7195=AXIS2_PLACEMENT_3D('',#11340,#8798,#8799);
#7196=AXIS2_PLACEMENT_3D('',#11346,#8803,#8804);
#7197=AXIS2_PLACEMENT_3D('',#11352,#8808,#8809);
#7198=AXIS2_PLACEMENT_3D('',#11358,#8813,#8814);
#7199=AXIS2_PLACEMENT_3D('',#11364,#8818,#8819);
#7200=AXIS2_PLACEMENT_3D('',#11370,#8823,#8824);
#7201=AXIS2_PLACEMENT_3D('',#11376,#8828,#8829);
#7202=AXIS2_PLACEMENT_3D('',#11382,#8833,#8834);
#7203=AXIS2_PLACEMENT_3D('',#11388,#8838,#8839);
#7204=AXIS2_PLACEMENT_3D('',#11394,#8843,#8844);
#7205=AXIS2_PLACEMENT_3D('',#11397,#8847,#8848);
#7206=AXIS2_PLACEMENT_3D('',#11398,#8849,#8850);
#7207=AXIS2_PLACEMENT_3D('',#11399,#8851,#8852);
#7208=AXIS2_PLACEMENT_3D('',#11400,#8853,#8854);
#7209=AXIS2_PLACEMENT_3D('',#11402,#8855,#8856);
#7210=AXIS2_PLACEMENT_3D('',#11405,#8858,#8859);
#7211=AXIS2_PLACEMENT_3D('',#11406,#8860,#8861);
#7212=AXIS2_PLACEMENT_3D('',#11410,#8863,#8864);
#7213=AXIS2_PLACEMENT_3D('',#11411,#8865,#8866);
#7214=AXIS2_PLACEMENT_3D('',#11428,#8867,#8868);
#7215=AXIS2_PLACEMENT_3D('',#11431,#8870,#8871);
#7216=AXIS2_PLACEMENT_3D('',#11433,#8872,#8873);
#7217=AXIS2_PLACEMENT_3D('',#11448,#8874,#8875);
#7218=AXIS2_PLACEMENT_3D('',#11449,#8876,#8877);
#7219=AXIS2_PLACEMENT_3D('',#11451,#8879,#8880);
#7220=AXIS2_PLACEMENT_3D('',#11454,#8881,#8882);
#7221=AXIS2_PLACEMENT_3D('',#11461,#8886,#8887);
#7222=AXIS2_PLACEMENT_3D('',#11463,#8888,#8889);
#7223=AXIS2_PLACEMENT_3D('',#11464,#8890,#8891);
#7224=AXIS2_PLACEMENT_3D('',#11470,#8895,#8896);
#7225=AXIS2_PLACEMENT_3D('',#11472,#8897,#8898);
#7226=AXIS2_PLACEMENT_3D('',#11476,#8901,#8902);
#7227=AXIS2_PLACEMENT_3D('',#11479,#8905,#8906);
#7228=AXIS2_PLACEMENT_3D('',#11480,#8907,#8908);
#7229=AXIS2_PLACEMENT_3D('',#11482,#8909,#8910);
#7230=AXIS2_PLACEMENT_3D('',#11484,#8912,#8913);
#7231=AXIS2_PLACEMENT_3D('',#11486,#8914,#8915);
#7232=AXIS2_PLACEMENT_3D('',#11488,#8917,#8918);
#7233=AXIS2_PLACEMENT_3D('',#11489,#8919,#8920);
#7234=AXIS2_PLACEMENT_3D('',#11490,#8921,#8922);
#7235=AXIS2_PLACEMENT_3D('',#11492,#8923,#8924);
#7236=AXIS2_PLACEMENT_3D('',#11495,#8926,#8927);
#7237=AXIS2_PLACEMENT_3D('',#11496,#8928,#8929);
#7238=AXIS2_PLACEMENT_3D('',#11497,#8930,#8931);
#7239=AXIS2_PLACEMENT_3D('',#11499,#8932,#8933);
#7240=AXIS2_PLACEMENT_3D('',#11502,#8935,#8936);
#7241=AXIS2_PLACEMENT_3D('',#11503,#8937,#8938);
#7242=AXIS2_PLACEMENT_3D('',#11504,#8939,#8940);
#7243=AXIS2_PLACEMENT_3D('',#11505,#8941,#8942);
#7244=AXIS2_PLACEMENT_3D('',#11506,#8943,#8944);
#7245=AXIS2_PLACEMENT_3D('',#11515,#8949,#8950);
#7246=AXIS2_PLACEMENT_3D('',#11521,#8954,#8955);
#7247=AXIS2_PLACEMENT_3D('',#11527,#8959,#8960);
#7248=AXIS2_PLACEMENT_3D('',#11533,#8964,#8965);
#7249=AXIS2_PLACEMENT_3D('',#11539,#8969,#8970);
#7250=AXIS2_PLACEMENT_3D('',#11542,#8973,#8974);
#7251=AXIS2_PLACEMENT_3D('',#11543,#8975,#8976);
#7252=AXIS2_PLACEMENT_3D('',#11545,#8977,#8978);
#7253=AXIS2_PLACEMENT_3D('',#11546,#8979,#8980);
#7254=AXIS2_PLACEMENT_3D('',#11548,#8981,#8982);
#7255=AXIS2_PLACEMENT_3D('',#11550,#8984,#8985);
#7256=AXIS2_PLACEMENT_3D('',#11552,#8986,#8987);
#7257=AXIS2_PLACEMENT_3D('',#11554,#8989,#8990);
#7258=AXIS2_PLACEMENT_3D('',#11556,#8991,#8992);
#7259=AXIS2_PLACEMENT_3D('',#11558,#8994,#8995);
#7260=AXIS2_PLACEMENT_3D('',#11559,#8996,#8997);
#7261=AXIS2_PLACEMENT_3D('',#11560,#8998,#8999);
#7262=AXIS2_PLACEMENT_3D('',#11562,#9000,#9001);
#7263=AXIS2_PLACEMENT_3D('',#11563,#9002,#9003);
#7264=AXIS2_PLACEMENT_3D('',#11565,#9004,#9005);
#7265=AXIS2_PLACEMENT_3D('',#11567,#9007,#9008);
#7266=AXIS2_PLACEMENT_3D('',#11569,#9009,#9010);
#7267=AXIS2_PLACEMENT_3D('',#11571,#9012,#9013);
#7268=AXIS2_PLACEMENT_3D('',#11573,#9014,#9015);
#7269=AXIS2_PLACEMENT_3D('',#11575,#9017,#9018);
#7270=AXIS2_PLACEMENT_3D('',#11577,#9019,#9020);
#7271=AXIS2_PLACEMENT_3D('',#11578,#9021,#9022);
#7272=AXIS2_PLACEMENT_3D('',#11580,#9023,#9024);
#7273=AXIS2_PLACEMENT_3D('',#11582,#9026,#9027);
#7274=AXIS2_PLACEMENT_3D('',#11584,#9028,#9029);
#7275=AXIS2_PLACEMENT_3D('',#11586,#9031,#9032);
#7276=AXIS2_PLACEMENT_3D('',#11588,#9033,#9034);
#7277=AXIS2_PLACEMENT_3D('',#11590,#9036,#9037);
#7278=AXIS2_PLACEMENT_3D('',#11591,#9038,#9039);
#7279=AXIS2_PLACEMENT_3D('',#11600,#9044,#9045);
#7280=AXIS2_PLACEMENT_3D('',#11606,#9049,#9050);
#7281=AXIS2_PLACEMENT_3D('',#11612,#9054,#9055);
#7282=AXIS2_PLACEMENT_3D('',#11618,#9059,#9060);
#7283=AXIS2_PLACEMENT_3D('',#11624,#9064,#9065);
#7284=AXIS2_PLACEMENT_3D('',#11627,#9068,#9069);
#7285=AXIS2_PLACEMENT_3D('',#11628,#9070,#9071);
#7286=AXIS2_PLACEMENT_3D('',#11629,#9072,#9073);
#7287=AXIS2_PLACEMENT_3D('',#11630,#9074,#9075);
#7288=AXIS2_PLACEMENT_3D('',#11631,#9076,#9077);
#7289=AXIS2_PLACEMENT_3D('',#11632,#9078,#9079);
#7290=AXIS2_PLACEMENT_3D('',#11633,#9080,#9081);
#7291=AXIS2_PLACEMENT_3D('',#11634,#9082,#9083);
#7292=AXIS2_PLACEMENT_3D('',#11635,#9084,#9085);
#7293=AXIS2_PLACEMENT_3D('',#11636,#9086,#9087);
#7294=AXIS2_PLACEMENT_3D('',#11637,#9088,#9089);
#7295=AXIS2_PLACEMENT_3D('',#11638,#9090,#9091);
#7296=AXIS2_PLACEMENT_3D('',#11639,#9092,#9093);
#7297=AXIS2_PLACEMENT_3D('',#11640,#9094,#9095);
#7298=AXIS2_PLACEMENT_3D('',#11641,#9096,#9097);
#7299=AXIS2_PLACEMENT_3D('',#11642,#9098,#9099);
#7300=AXIS2_PLACEMENT_3D('',#11643,#9100,#9101);
#7301=AXIS2_PLACEMENT_3D('',#11644,#9102,#9103);
#7302=AXIS2_PLACEMENT_3D('',#11645,#9104,#9105);
#7303=AXIS2_PLACEMENT_3D('',#11646,#9106,#9107);
#7304=AXIS2_PLACEMENT_3D('',#11647,#9108,#9109);
#7305=AXIS2_PLACEMENT_3D('',#11648,#9110,#9111);
#7306=AXIS2_PLACEMENT_3D('',#11649,#9112,#9113);
#7307=AXIS2_PLACEMENT_3D('',#11650,#9114,#9115);
#7308=AXIS2_PLACEMENT_3D('',#11651,#9116,#9117);
#7309=AXIS2_PLACEMENT_3D('',#11652,#9118,#9119);
#7310=AXIS2_PLACEMENT_3D('',#11653,#9120,#9121);
#7311=AXIS2_PLACEMENT_3D('',#11654,#9122,#9123);
#7312=AXIS2_PLACEMENT_3D('',#11655,#9124,#9125);
#7313=AXIS2_PLACEMENT_3D('',#11656,#9126,#9127);
#7314=AXIS2_PLACEMENT_3D('',#11657,#9128,#9129);
#7315=AXIS2_PLACEMENT_3D('',#11658,#9130,#9131);
#7316=AXIS2_PLACEMENT_3D('',#11659,#9132,#9133);
#7317=AXIS2_PLACEMENT_3D('',#11660,#9134,#9135);
#7318=AXIS2_PLACEMENT_3D('',#11661,#9136,#9137);
#7319=AXIS2_PLACEMENT_3D('',#11662,#9138,#9139);
#7320=AXIS2_PLACEMENT_3D('',#11663,#9140,#9141);
#7321=AXIS2_PLACEMENT_3D('',#11664,#9142,#9143);
#7322=AXIS2_PLACEMENT_3D('',#11665,#9144,#9145);
#7323=AXIS2_PLACEMENT_3D('',#11666,#9146,#9147);
#7324=AXIS2_PLACEMENT_3D('',#11667,#9148,#9149);
#7325=AXIS2_PLACEMENT_3D('',#11668,#9150,#9151);
#7326=AXIS2_PLACEMENT_3D('',#11669,#9152,#9153);
#7327=AXIS2_PLACEMENT_3D('',#11670,#9154,#9155);
#7328=AXIS2_PLACEMENT_3D('',#11671,#9156,#9157);
#7329=AXIS2_PLACEMENT_3D('',#11672,#9158,#9159);
#7330=AXIS2_PLACEMENT_3D('',#11673,#9160,#9161);
#7331=AXIS2_PLACEMENT_3D('',#11674,#9162,#9163);
#7332=AXIS2_PLACEMENT_3D('',#11675,#9164,#9165);
#7333=AXIS2_PLACEMENT_3D('',#11676,#9166,#9167);
#7334=AXIS2_PLACEMENT_3D('',#11677,#9168,#9169);
#7335=AXIS2_PLACEMENT_3D('',#11678,#9170,#9171);
#7336=AXIS2_PLACEMENT_3D('',#11679,#9172,#9173);
#7337=AXIS2_PLACEMENT_3D('',#11680,#9174,#9175);
#7338=AXIS2_PLACEMENT_3D('',#11681,#9176,#9177);
#7339=AXIS2_PLACEMENT_3D('',#11682,#9178,#9179);
#7340=AXIS2_PLACEMENT_3D('',#11683,#9180,#9181);
#7341=AXIS2_PLACEMENT_3D('',#11684,#9182,#9183);
#7342=AXIS2_PLACEMENT_3D('',#11685,#9184,#9185);
#7343=AXIS2_PLACEMENT_3D('',#11686,#9186,#9187);
#7344=AXIS2_PLACEMENT_3D('',#11688,#9188,#9189);
#7345=AXIS2_PLACEMENT_3D('',#11691,#9191,#9192);
#7346=AXIS2_PLACEMENT_3D('',#11692,#9193,#9194);
#7347=AXIS2_PLACEMENT_3D('',#11697,#9196,#9197);
#7348=AXIS2_PLACEMENT_3D('',#11700,#9199,#9200);
#7349=AXIS2_PLACEMENT_3D('',#11701,#9201,#9202);
#7350=AXIS2_PLACEMENT_3D('',#11707,#9206,#9207);
#7351=AXIS2_PLACEMENT_3D('',#11711,#9210,#9211);
#7352=AXIS2_PLACEMENT_3D('',#11715,#9214,#9215);
#7353=AXIS2_PLACEMENT_3D('',#11717,#9217,#9218);
#7354=AXIS2_PLACEMENT_3D('',#11718,#9219,#9220);
#7355=AXIS2_PLACEMENT_3D('',#11719,#9221,#9222);
#7356=AXIS2_PLACEMENT_3D('',#11720,#9223,#9224);
#7357=AXIS2_PLACEMENT_3D('',#11721,#9225,#9226);
#7358=DIRECTION('axis',(0.,0.,1.));
#7359=DIRECTION('refdir',(1.,0.,0.));
#7360=DIRECTION('axis',(0.,0.,1.));
#7361=DIRECTION('refdir',(1.,0.,0.));
#7362=DIRECTION('axis',(0.,0.,1.));
#7363=DIRECTION('refdir',(1.,0.,0.));
#7364=DIRECTION('center_axis',(0.,0.,1.));
#7365=DIRECTION('ref_axis',(1.,0.,0.));
#7366=DIRECTION('center_axis',(0.,0.,1.));
#7367=DIRECTION('ref_axis',(1.,0.,0.));
#7368=DIRECTION('',(0.,0.,1.));
#7369=DIRECTION('center_axis',(0.,0.,-1.));
#7370=DIRECTION('ref_axis',(1.,0.,0.));
#7371=DIRECTION('center_axis',(0.,0.,1.));
#7372=DIRECTION('ref_axis',(1.,0.,0.));
#7373=DIRECTION('center_axis',(0.,0.,1.));
#7374=DIRECTION('ref_axis',(1.,0.,0.));
#7375=DIRECTION('',(0.,0.,1.));
#7376=DIRECTION('center_axis',(0.,0.,-1.));
#7377=DIRECTION('ref_axis',(1.,0.,0.));
#7378=DIRECTION('center_axis',(0.,0.,1.));
#7379=DIRECTION('ref_axis',(1.,0.,0.));
#7380=DIRECTION('center_axis',(0.,0.,1.));
#7381=DIRECTION('ref_axis',(1.,0.,0.));
#7382=DIRECTION('',(0.,0.,1.));
#7383=DIRECTION('center_axis',(0.,0.,-1.));
#7384=DIRECTION('ref_axis',(1.,0.,0.));
#7385=DIRECTION('center_axis',(0.,0.,1.));
#7386=DIRECTION('ref_axis',(1.,0.,0.));
#7387=DIRECTION('center_axis',(0.,0.,1.));
#7388=DIRECTION('ref_axis',(1.,0.,0.));
#7389=DIRECTION('',(0.,0.,1.));
#7390=DIRECTION('center_axis',(0.,0.,-1.));
#7391=DIRECTION('ref_axis',(1.,0.,0.));
#7392=DIRECTION('center_axis',(0.,0.,1.));
#7393=DIRECTION('ref_axis',(1.,0.,0.));
#7394=DIRECTION('center_axis',(0.,0.,1.));
#7395=DIRECTION('ref_axis',(1.,0.,0.));
#7396=DIRECTION('',(0.,0.,1.));
#7397=DIRECTION('center_axis',(0.,0.,-1.));
#7398=DIRECTION('ref_axis',(1.,0.,0.));
#7399=DIRECTION('center_axis',(0.,0.,1.));
#7400=DIRECTION('ref_axis',(1.,0.,0.));
#7401=DIRECTION('center_axis',(0.,0.,1.));
#7402=DIRECTION('ref_axis',(1.,0.,0.));
#7403=DIRECTION('',(0.,0.,1.));
#7404=DIRECTION('center_axis',(0.,0.,-1.));
#7405=DIRECTION('ref_axis',(1.,0.,0.));
#7406=DIRECTION('center_axis',(0.,0.,1.));
#7407=DIRECTION('ref_axis',(1.,0.,0.));
#7408=DIRECTION('center_axis',(0.,0.,1.));
#7409=DIRECTION('ref_axis',(1.,0.,0.));
#7410=DIRECTION('',(0.,0.,1.));
#7411=DIRECTION('center_axis',(0.,0.,-1.));
#7412=DIRECTION('ref_axis',(1.,0.,0.));
#7413=DIRECTION('center_axis',(0.,0.,1.));
#7414=DIRECTION('ref_axis',(1.,0.,0.));
#7415=DIRECTION('center_axis',(0.,0.,1.));
#7416=DIRECTION('ref_axis',(1.,0.,0.));
#7417=DIRECTION('',(0.,0.,1.));
#7418=DIRECTION('center_axis',(0.,0.,-1.));
#7419=DIRECTION('ref_axis',(1.,0.,0.));
#7420=DIRECTION('center_axis',(0.,0.,1.));
#7421=DIRECTION('ref_axis',(1.,0.,0.));
#7422=DIRECTION('center_axis',(0.,0.,1.));
#7423=DIRECTION('ref_axis',(1.,0.,0.));
#7424=DIRECTION('',(0.,0.,1.));
#7425=DIRECTION('center_axis',(0.,0.,-1.));
#7426=DIRECTION('ref_axis',(1.,0.,0.));
#7427=DIRECTION('center_axis',(0.,0.,1.));
#7428=DIRECTION('ref_axis',(1.,0.,0.));
#7429=DIRECTION('center_axis',(0.,0.,1.));
#7430=DIRECTION('ref_axis',(1.,0.,0.));
#7431=DIRECTION('',(0.,0.,1.));
#7432=DIRECTION('center_axis',(0.,0.,-1.));
#7433=DIRECTION('ref_axis',(1.,0.,0.));
#7434=DIRECTION('center_axis',(0.,1.,0.));
#7435=DIRECTION('ref_axis',(-1.,0.,0.));
#7436=DIRECTION('',(-1.,0.,0.));
#7437=DIRECTION('',(0.,0.,1.));
#7438=DIRECTION('',(-1.,0.,0.));
#7439=DIRECTION('',(0.,0.,1.));
#7440=DIRECTION('center_axis',(1.,0.,0.));
#7441=DIRECTION('ref_axis',(0.,1.,0.));
#7442=DIRECTION('',(0.,1.,0.));
#7443=DIRECTION('',(0.,1.,0.));
#7444=DIRECTION('',(0.,0.,1.));
#7445=DIRECTION('center_axis',(0.,-1.,0.));
#7446=DIRECTION('ref_axis',(1.,0.,0.));
#7447=DIRECTION('',(1.,0.,0.));
#7448=DIRECTION('',(1.,0.,0.));
#7449=DIRECTION('',(0.,0.,1.));
#7450=DIRECTION('center_axis',(-1.,0.,0.));
#7451=DIRECTION('ref_axis',(0.,-1.,0.));
#7452=DIRECTION('',(0.,-1.,0.));
#7453=DIRECTION('',(0.,-1.,0.));
#7454=DIRECTION('center_axis',(0.,0.,1.));
#7455=DIRECTION('ref_axis',(1.,0.,0.));
#7456=DIRECTION('center_axis',(0.,0.,1.));
#7457=DIRECTION('ref_axis',(1.,0.,0.));
#7458=DIRECTION('axis',(0.,0.,1.));
#7459=DIRECTION('refdir',(1.,0.,0.));
#7460=DIRECTION('center_axis',(0.,1.,0.));
#7461=DIRECTION('ref_axis',(-1.,0.,0.));
#7462=DIRECTION('',(-1.,0.,0.));
#7463=DIRECTION('',(0.,0.,1.));
#7464=DIRECTION('',(-1.,0.,0.));
#7465=DIRECTION('',(0.,0.,1.));
#7466=DIRECTION('center_axis',(1.,0.,0.));
#7467=DIRECTION('ref_axis',(0.,1.,0.));
#7468=DIRECTION('',(0.,1.,0.));
#7469=DIRECTION('',(0.,1.,0.));
#7470=DIRECTION('',(0.,0.,1.));
#7471=DIRECTION('center_axis',(0.,-1.,0.));
#7472=DIRECTION('ref_axis',(1.,0.,0.));
#7473=DIRECTION('',(1.,0.,0.));
#7474=DIRECTION('',(1.,0.,0.));
#7475=DIRECTION('',(0.,0.,1.));
#7476=DIRECTION('center_axis',(-1.,0.,0.));
#7477=DIRECTION('ref_axis',(0.,-1.,0.));
#7478=DIRECTION('',(0.,-1.,0.));
#7479=DIRECTION('',(0.,-1.,0.));
#7480=DIRECTION('center_axis',(0.,0.,1.));
#7481=DIRECTION('ref_axis',(1.,0.,0.));
#7482=DIRECTION('center_axis',(0.,0.,1.));
#7483=DIRECTION('ref_axis',(1.,0.,0.));
#7484=DIRECTION('axis',(0.,0.,1.));
#7485=DIRECTION('refdir',(1.,0.,0.));
#7486=DIRECTION('center_axis',(0.,1.,0.));
#7487=DIRECTION('ref_axis',(-1.,0.,0.));
#7488=DIRECTION('',(-1.,0.,0.));
#7489=DIRECTION('',(0.,0.,1.));
#7490=DIRECTION('',(-1.,0.,0.));
#7491=DIRECTION('',(0.,0.,1.));
#7492=DIRECTION('center_axis',(1.,0.,0.));
#7493=DIRECTION('ref_axis',(0.,1.,0.));
#7494=DIRECTION('',(0.,1.,0.));
#7495=DIRECTION('',(0.,1.,0.));
#7496=DIRECTION('',(0.,0.,1.));
#7497=DIRECTION('center_axis',(0.,-1.,0.));
#7498=DIRECTION('ref_axis',(1.,0.,0.));
#7499=DIRECTION('',(1.,0.,0.));
#7500=DIRECTION('',(1.,0.,0.));
#7501=DIRECTION('',(0.,0.,1.));
#7502=DIRECTION('center_axis',(-1.,0.,0.));
#7503=DIRECTION('ref_axis',(0.,-1.,0.));
#7504=DIRECTION('',(0.,-1.,0.));
#7505=DIRECTION('',(0.,-1.,0.));
#7506=DIRECTION('center_axis',(0.,0.,1.));
#7507=DIRECTION('ref_axis',(1.,0.,0.));
#7508=DIRECTION('center_axis',(0.,0.,1.));
#7509=DIRECTION('ref_axis',(1.,0.,0.));
#7510=DIRECTION('axis',(0.,0.,1.));
#7511=DIRECTION('refdir',(1.,0.,0.));
#7512=DIRECTION('center_axis',(0.,0.,1.));
#7513=DIRECTION('ref_axis',(1.,0.,0.));
#7514=DIRECTION('center_axis',(0.,0.,1.));
#7515=DIRECTION('ref_axis',(1.,0.,0.));
#7516=DIRECTION('',(0.,0.,1.));
#7517=DIRECTION('center_axis',(0.,0.,-1.));
#7518=DIRECTION('ref_axis',(1.,0.,0.));
#7519=DIRECTION('center_axis',(0.,0.,1.));
#7520=DIRECTION('ref_axis',(1.,0.,0.));
#7521=DIRECTION('center_axis',(0.,0.,1.));
#7522=DIRECTION('ref_axis',(1.,0.,0.));
#7523=DIRECTION('center_axis',(0.,0.,1.));
#7524=DIRECTION('ref_axis',(1.,0.,0.));
#7525=DIRECTION('center_axis',(0.,0.,1.));
#7526=DIRECTION('ref_axis',(1.,0.,0.));
#7527=DIRECTION('',(0.,0.,1.));
#7528=DIRECTION('center_axis',(0.,0.,-1.));
#7529=DIRECTION('ref_axis',(1.,0.,0.));
#7530=DIRECTION('center_axis',(0.,0.,1.));
#7531=DIRECTION('ref_axis',(1.,0.,0.));
#7532=DIRECTION('center_axis',(0.,0.,1.));
#7533=DIRECTION('ref_axis',(1.,0.,0.));
#7534=DIRECTION('center_axis',(0.,0.,1.));
#7535=DIRECTION('ref_axis',(1.,0.,0.));
#7536=DIRECTION('center_axis',(0.,0.,1.));
#7537=DIRECTION('ref_axis',(1.,0.,0.));
#7538=DIRECTION('',(0.,0.,1.));
#7539=DIRECTION('center_axis',(0.,0.,1.));
#7540=DIRECTION('ref_axis',(1.,0.,0.));
#7541=DIRECTION('center_axis',(0.,0.,1.));
#7542=DIRECTION('ref_axis',(1.,0.,0.));
#7543=DIRECTION('',(0.,0.,1.));
#7544=DIRECTION('center_axis',(0.,0.,1.));
#7545=DIRECTION('ref_axis',(1.,0.,0.));
#7546=DIRECTION('center_axis',(0.,0.,1.));
#7547=DIRECTION('ref_axis',(1.,0.,0.));
#7548=DIRECTION('',(0.,0.,1.));
#7549=DIRECTION('center_axis',(0.,0.,-1.));
#7550=DIRECTION('ref_axis',(1.,0.,0.));
#7551=DIRECTION('center_axis',(0.,0.,1.));
#7552=DIRECTION('ref_axis',(1.,0.,0.));
#7553=DIRECTION('center_axis',(0.,0.,1.));
#7554=DIRECTION('ref_axis',(1.,0.,0.));
#7555=DIRECTION('center_axis',(0.,0.,1.));
#7556=DIRECTION('ref_axis',(1.,0.,0.));
#7557=DIRECTION('center_axis',(0.,0.,1.));
#7558=DIRECTION('ref_axis',(1.,0.,0.));
#7559=DIRECTION('',(0.,0.,1.));
#7560=DIRECTION('center_axis',(0.,0.,-1.));
#7561=DIRECTION('ref_axis',(1.,0.,0.));
#7562=DIRECTION('center_axis',(0.,0.,1.));
#7563=DIRECTION('ref_axis',(1.,0.,0.));
#7564=DIRECTION('center_axis',(0.,0.,1.));
#7565=DIRECTION('ref_axis',(1.,0.,0.));
#7566=DIRECTION('center_axis',(0.,0.,1.));
#7567=DIRECTION('ref_axis',(1.,0.,0.));
#7568=DIRECTION('center_axis',(0.,0.,1.));
#7569=DIRECTION('ref_axis',(1.,0.,0.));
#7570=DIRECTION('',(0.,0.,1.));
#7571=DIRECTION('center_axis',(0.,0.,1.));
#7572=DIRECTION('ref_axis',(1.,0.,0.));
#7573=DIRECTION('center_axis',(0.,0.,1.));
#7574=DIRECTION('ref_axis',(1.,0.,0.));
#7575=DIRECTION('',(0.,0.,1.));
#7576=DIRECTION('center_axis',(0.,0.,1.));
#7577=DIRECTION('ref_axis',(1.,0.,0.));
#7578=DIRECTION('center_axis',(0.,0.,1.));
#7579=DIRECTION('ref_axis',(1.,0.,0.));
#7580=DIRECTION('',(0.,0.,1.));
#7581=DIRECTION('center_axis',(0.,0.,-1.));
#7582=DIRECTION('ref_axis',(1.,0.,0.));
#7583=DIRECTION('center_axis',(0.,0.,1.));
#7584=DIRECTION('ref_axis',(1.,0.,0.));
#7585=DIRECTION('center_axis',(0.,0.,1.));
#7586=DIRECTION('ref_axis',(1.,0.,0.));
#7587=DIRECTION('',(0.,0.,1.));
#7588=DIRECTION('center_axis',(0.,0.,-1.));
#7589=DIRECTION('ref_axis',(1.,0.,0.));
#7590=DIRECTION('center_axis',(0.,1.,0.));
#7591=DIRECTION('ref_axis',(-1.,0.,0.));
#7592=DIRECTION('',(-1.,0.,0.));
#7593=DIRECTION('',(0.,0.,1.));
#7594=DIRECTION('',(-1.,0.,0.));
#7595=DIRECTION('',(0.,0.,1.));
#7596=DIRECTION('center_axis',(1.,0.,0.));
#7597=DIRECTION('ref_axis',(0.,1.,0.));
#7598=DIRECTION('',(0.,1.,0.));
#7599=DIRECTION('',(0.,1.,0.));
#7600=DIRECTION('',(0.,0.,1.));
#7601=DIRECTION('center_axis',(0.,-1.,0.));
#7602=DIRECTION('ref_axis',(1.,0.,0.));
#7603=DIRECTION('',(1.,0.,0.));
#7604=DIRECTION('',(1.,0.,0.));
#7605=DIRECTION('',(0.,0.,1.));
#7606=DIRECTION('center_axis',(-1.,0.,0.));
#7607=DIRECTION('ref_axis',(0.,-1.,0.));
#7608=DIRECTION('',(0.,-1.,0.));
#7609=DIRECTION('',(0.,-1.,0.));
#7610=DIRECTION('center_axis',(0.,0.,1.));
#7611=DIRECTION('ref_axis',(1.,0.,0.));
#7612=DIRECTION('center_axis',(0.,0.,1.));
#7613=DIRECTION('ref_axis',(1.,0.,0.));
#7614=DIRECTION('axis',(0.,0.,1.));
#7615=DIRECTION('refdir',(1.,0.,0.));
#7616=DIRECTION('center_axis',(0.,0.,1.));
#7617=DIRECTION('ref_axis',(1.,0.,0.));
#7618=DIRECTION('center_axis',(0.,0.,-1.));
#7619=DIRECTION('ref_axis',(1.,0.,0.));
#7620=DIRECTION('',(0.,0.,-1.));
#7621=DIRECTION('center_axis',(0.,0.,-1.));
#7622=DIRECTION('ref_axis',(1.,0.,0.));
#7623=DIRECTION('center_axis',(0.,0.,1.));
#7624=DIRECTION('ref_axis',(1.,0.,0.));
#7625=DIRECTION('center_axis',(0.,0.,1.));
#7626=DIRECTION('ref_axis',(1.,0.,0.));
#7627=DIRECTION('',(0.,0.,-1.));
#7628=DIRECTION('center_axis',(0.,0.,1.));
#7629=DIRECTION('ref_axis',(1.,0.,0.));
#7630=DIRECTION('center_axis',(0.,0.,1.));
#7631=DIRECTION('ref_axis',(1.,0.,0.));
#7632=DIRECTION('center_axis',(0.,0.,1.));
#7633=DIRECTION('ref_axis',(1.,0.,0.));
#7634=DIRECTION('axis',(0.,0.,1.));
#7635=DIRECTION('refdir',(1.,0.,0.));
#7636=DIRECTION('center_axis',(0.,0.,1.));
#7637=DIRECTION('ref_axis',(1.,0.,0.));
#7638=DIRECTION('center_axis',(0.,0.,-1.));
#7639=DIRECTION('ref_axis',(1.,0.,0.));
#7640=DIRECTION('',(0.,0.,-1.));
#7641=DIRECTION('center_axis',(0.,0.,-1.));
#7642=DIRECTION('ref_axis',(1.,0.,0.));
#7643=DIRECTION('center_axis',(0.,0.,1.));
#7644=DIRECTION('ref_axis',(1.,0.,0.));
#7645=DIRECTION('center_axis',(0.,0.,1.));
#7646=DIRECTION('ref_axis',(1.,0.,0.));
#7647=DIRECTION('',(0.,0.,-1.));
#7648=DIRECTION('center_axis',(0.,0.,1.));
#7649=DIRECTION('ref_axis',(1.,0.,0.));
#7650=DIRECTION('center_axis',(0.,0.,1.));
#7651=DIRECTION('ref_axis',(1.,0.,0.));
#7652=DIRECTION('center_axis',(0.,0.,1.));
#7653=DIRECTION('ref_axis',(1.,0.,0.));
#7654=DIRECTION('axis',(0.,0.,1.));
#7655=DIRECTION('refdir',(1.,0.,0.));
#7656=DIRECTION('center_axis',(0.,0.,1.));
#7657=DIRECTION('ref_axis',(1.,0.,0.));
#7658=DIRECTION('center_axis',(0.,0.,1.));
#7659=DIRECTION('ref_axis',(1.,0.,0.));
#7660=DIRECTION('',(0.,0.,1.));
#7661=DIRECTION('center_axis',(0.,0.,-1.));
#7662=DIRECTION('ref_axis',(1.,0.,0.));
#7663=DIRECTION('center_axis',(0.,0.,1.));
#7664=DIRECTION('ref_axis',(1.,0.,0.));
#7665=DIRECTION('center_axis',(0.,0.,1.));
#7666=DIRECTION('ref_axis',(1.,0.,0.));
#7667=DIRECTION('center_axis',(0.,0.,1.));
#7668=DIRECTION('ref_axis',(1.,0.,0.));
#7669=DIRECTION('center_axis',(0.,0.,1.));
#7670=DIRECTION('ref_axis',(1.,0.,0.));
#7671=DIRECTION('',(0.,0.,1.));
#7672=DIRECTION('center_axis',(0.,0.,-1.));
#7673=DIRECTION('ref_axis',(1.,0.,0.));
#7674=DIRECTION('center_axis',(0.,0.,1.));
#7675=DIRECTION('ref_axis',(1.,0.,0.));
#7676=DIRECTION('center_axis',(0.,0.,1.));
#7677=DIRECTION('ref_axis',(1.,0.,0.));
#7678=DIRECTION('center_axis',(0.,0.,1.));
#7679=DIRECTION('ref_axis',(1.,0.,0.));
#7680=DIRECTION('center_axis',(0.,0.,1.));
#7681=DIRECTION('ref_axis',(1.,0.,0.));
#7682=DIRECTION('',(0.,0.,1.));
#7683=DIRECTION('center_axis',(0.,0.,1.));
#7684=DIRECTION('ref_axis',(1.,0.,0.));
#7685=DIRECTION('center_axis',(0.,0.,1.));
#7686=DIRECTION('ref_axis',(1.,0.,0.));
#7687=DIRECTION('',(0.,0.,1.));
#7688=DIRECTION('center_axis',(0.,0.,1.));
#7689=DIRECTION('ref_axis',(1.,0.,0.));
#7690=DIRECTION('center_axis',(0.,0.,1.));
#7691=DIRECTION('ref_axis',(1.,0.,0.));
#7692=DIRECTION('',(0.,0.,1.));
#7693=DIRECTION('center_axis',(0.,0.,-1.));
#7694=DIRECTION('ref_axis',(1.,0.,0.));
#7695=DIRECTION('center_axis',(0.,0.,1.));
#7696=DIRECTION('ref_axis',(1.,0.,0.));
#7697=DIRECTION('center_axis',(0.,0.,1.));
#7698=DIRECTION('ref_axis',(1.,0.,0.));
#7699=DIRECTION('center_axis',(0.,0.,1.));
#7700=DIRECTION('ref_axis',(1.,0.,0.));
#7701=DIRECTION('center_axis',(0.,0.,1.));
#7702=DIRECTION('ref_axis',(1.,0.,0.));
#7703=DIRECTION('',(0.,0.,1.));
#7704=DIRECTION('center_axis',(0.,0.,-1.));
#7705=DIRECTION('ref_axis',(1.,0.,0.));
#7706=DIRECTION('center_axis',(0.,0.,1.));
#7707=DIRECTION('ref_axis',(1.,0.,0.));
#7708=DIRECTION('center_axis',(0.,0.,1.));
#7709=DIRECTION('ref_axis',(1.,0.,0.));
#7710=DIRECTION('center_axis',(0.,0.,1.));
#7711=DIRECTION('ref_axis',(1.,0.,0.));
#7712=DIRECTION('center_axis',(0.,0.,1.));
#7713=DIRECTION('ref_axis',(1.,0.,0.));
#7714=DIRECTION('',(0.,0.,1.));
#7715=DIRECTION('center_axis',(0.,0.,1.));
#7716=DIRECTION('ref_axis',(1.,0.,0.));
#7717=DIRECTION('center_axis',(0.,0.,1.));
#7718=DIRECTION('ref_axis',(1.,0.,0.));
#7719=DIRECTION('',(0.,0.,1.));
#7720=DIRECTION('center_axis',(0.,0.,1.));
#7721=DIRECTION('ref_axis',(1.,0.,0.));
#7722=DIRECTION('center_axis',(0.,0.,1.));
#7723=DIRECTION('ref_axis',(1.,0.,0.));
#7724=DIRECTION('',(0.,0.,1.));
#7725=DIRECTION('center_axis',(0.,0.,-1.));
#7726=DIRECTION('ref_axis',(1.,0.,0.));
#7727=DIRECTION('center_axis',(0.,0.,1.));
#7728=DIRECTION('ref_axis',(1.,0.,0.));
#7729=DIRECTION('center_axis',(0.,0.,1.));
#7730=DIRECTION('ref_axis',(1.,0.,0.));
#7731=DIRECTION('',(0.,0.,1.));
#7732=DIRECTION('center_axis',(0.,0.,-1.));
#7733=DIRECTION('ref_axis',(1.,0.,0.));
#7734=DIRECTION('center_axis',(0.,1.,0.));
#7735=DIRECTION('ref_axis',(-1.,0.,0.));
#7736=DIRECTION('',(-1.,0.,0.));
#7737=DIRECTION('',(0.,0.,1.));
#7738=DIRECTION('',(-1.,0.,0.));
#7739=DIRECTION('',(0.,0.,1.));
#7740=DIRECTION('center_axis',(1.,0.,0.));
#7741=DIRECTION('ref_axis',(0.,1.,0.));
#7742=DIRECTION('',(0.,1.,0.));
#7743=DIRECTION('',(0.,1.,0.));
#7744=DIRECTION('',(0.,0.,1.));
#7745=DIRECTION('center_axis',(0.,-1.,0.));
#7746=DIRECTION('ref_axis',(1.,0.,0.));
#7747=DIRECTION('',(1.,0.,0.));
#7748=DIRECTION('',(1.,0.,0.));
#7749=DIRECTION('',(0.,0.,1.));
#7750=DIRECTION('center_axis',(-1.,0.,0.));
#7751=DIRECTION('ref_axis',(0.,-1.,0.));
#7752=DIRECTION('',(0.,-1.,0.));
#7753=DIRECTION('',(0.,-1.,0.));
#7754=DIRECTION('center_axis',(0.,0.,1.));
#7755=DIRECTION('ref_axis',(1.,0.,0.));
#7756=DIRECTION('center_axis',(0.,0.,1.));
#7757=DIRECTION('ref_axis',(1.,0.,0.));
#7758=DIRECTION('axis',(0.,0.,1.));
#7759=DIRECTION('refdir',(1.,0.,0.));
#7760=DIRECTION('center_axis',(0.,0.,1.));
#7761=DIRECTION('ref_axis',(1.,0.,0.));
#7762=DIRECTION('center_axis',(0.,0.,-1.));
#7763=DIRECTION('ref_axis',(1.,0.,0.));
#7764=DIRECTION('',(0.,0.,-1.));
#7765=DIRECTION('center_axis',(0.,0.,-1.));
#7766=DIRECTION('ref_axis',(1.,0.,0.));
#7767=DIRECTION('center_axis',(0.,0.,1.));
#7768=DIRECTION('ref_axis',(1.,0.,0.));
#7769=DIRECTION('center_axis',(0.,0.,1.));
#7770=DIRECTION('ref_axis',(1.,0.,0.));
#7771=DIRECTION('',(0.,0.,-1.));
#7772=DIRECTION('center_axis',(0.,0.,1.));
#7773=DIRECTION('ref_axis',(1.,0.,0.));
#7774=DIRECTION('center_axis',(0.,0.,1.));
#7775=DIRECTION('ref_axis',(1.,0.,0.));
#7776=DIRECTION('center_axis',(0.,0.,1.));
#7777=DIRECTION('ref_axis',(1.,0.,0.));
#7778=DIRECTION('axis',(0.,0.,1.));
#7779=DIRECTION('refdir',(1.,0.,0.));
#7780=DIRECTION('center_axis',(0.,0.,1.));
#7781=DIRECTION('ref_axis',(1.,0.,0.));
#7782=DIRECTION('center_axis',(0.,0.,-1.));
#7783=DIRECTION('ref_axis',(1.,0.,0.));
#7784=DIRECTION('',(0.,0.,-1.));
#7785=DIRECTION('center_axis',(0.,0.,-1.));
#7786=DIRECTION('ref_axis',(1.,0.,0.));
#7787=DIRECTION('center_axis',(0.,0.,1.));
#7788=DIRECTION('ref_axis',(1.,0.,0.));
#7789=DIRECTION('center_axis',(0.,0.,1.));
#7790=DIRECTION('ref_axis',(1.,0.,0.));
#7791=DIRECTION('',(0.,0.,-1.));
#7792=DIRECTION('center_axis',(0.,0.,1.));
#7793=DIRECTION('ref_axis',(1.,0.,0.));
#7794=DIRECTION('center_axis',(0.,0.,1.));
#7795=DIRECTION('ref_axis',(1.,0.,0.));
#7796=DIRECTION('center_axis',(0.,0.,1.));
#7797=DIRECTION('ref_axis',(1.,0.,0.));
#7798=DIRECTION('axis',(0.,0.,1.));
#7799=DIRECTION('refdir',(1.,0.,0.));
#7800=DIRECTION('center_axis',(0.,0.,1.));
#7801=DIRECTION('ref_axis',(1.,0.,0.));
#7802=DIRECTION('center_axis',(0.,0.,1.));
#7803=DIRECTION('ref_axis',(1.,0.,0.));
#7804=DIRECTION('',(0.,0.,1.));
#7805=DIRECTION('center_axis',(0.,0.,-1.));
#7806=DIRECTION('ref_axis',(1.,0.,0.));
#7807=DIRECTION('center_axis',(0.,0.,1.));
#7808=DIRECTION('ref_axis',(1.,0.,0.));
#7809=DIRECTION('center_axis',(0.,0.,1.));
#7810=DIRECTION('ref_axis',(1.,0.,0.));
#7811=DIRECTION('',(0.,0.,1.));
#7812=DIRECTION('center_axis',(0.,0.,-1.));
#7813=DIRECTION('ref_axis',(1.,0.,0.));
#7814=DIRECTION('center_axis',(0.,1.,0.));
#7815=DIRECTION('ref_axis',(1.,0.,0.));
#7816=DIRECTION('center_axis',(0.,1.,0.));
#7817=DIRECTION('ref_axis',(1.,0.,0.));
#7818=DIRECTION('',(0.,1.,0.));
#7819=DIRECTION('center_axis',(0.,-1.,0.));
#7820=DIRECTION('ref_axis',(1.,0.,0.));
#7821=DIRECTION('center_axis',(0.,0.,1.));
#7822=DIRECTION('ref_axis',(1.,0.,0.));
#7823=DIRECTION('',(-1.,0.,0.));
#7824=DIRECTION('',(0.,1.,0.));
#7825=DIRECTION('',(1.,0.,0.));
#7826=DIRECTION('',(0.,1.,0.));
#7827=DIRECTION('',(-1.,0.,0.));
#7828=DIRECTION('',(0.,1.,0.));
#7829=DIRECTION('',(1.,0.,0.));
#7830=DIRECTION('',(0.,-1.,0.));
#7831=DIRECTION('center_axis',(-1.,0.,0.));
#7832=DIRECTION('ref_axis',(0.,0.,1.));
#7833=DIRECTION('',(0.,0.,-1.));
#7834=DIRECTION('',(0.,0.,1.));
#7835=DIRECTION('',(0.,1.,0.));
#7836=DIRECTION('center_axis',(1.,0.,0.));
#7837=DIRECTION('ref_axis',(0.,0.,-1.));
#7838=DIRECTION('',(0.,0.,1.));
#7839=DIRECTION('',(0.,1.,0.));
#7840=DIRECTION('',(0.,0.,-1.));
#7841=DIRECTION('center_axis',(0.,1.,0.));
#7842=DIRECTION('ref_axis',(0.,0.,1.));
#7843=DIRECTION('',(-1.,0.,0.));
#7844=DIRECTION('center_axis',(0.,1.,0.));
#7845=DIRECTION('ref_axis',(1.,0.,0.));
#7846=DIRECTION('',(1.,0.,0.));
#7847=DIRECTION('center_axis',(0.,-1.,0.));
#7848=DIRECTION('ref_axis',(1.,0.,0.));
#7849=DIRECTION('',(0.,0.,1.));
#7850=DIRECTION('',(1.,0.,0.));
#7851=DIRECTION('',(0.,0.,1.));
#7852=DIRECTION('center_axis',(1.,0.,0.));
#7853=DIRECTION('ref_axis',(0.,1.,0.));
#7854=DIRECTION('',(0.,0.,1.));
#7855=DIRECTION('',(0.,1.,0.));
#7856=DIRECTION('center_axis',(0.,1.,0.));
#7857=DIRECTION('ref_axis',(-1.,0.,0.));
#7858=DIRECTION('',(0.,0.,1.));
#7859=DIRECTION('',(-1.,0.,0.));
#7860=DIRECTION('center_axis',(-1.,0.,0.));
#7861=DIRECTION('ref_axis',(0.,-1.,0.));
#7862=DIRECTION('',(0.,-1.,0.));
#7863=DIRECTION('center_axis',(0.,0.,1.));
#7864=DIRECTION('ref_axis',(1.,0.,0.));
#7865=DIRECTION('center_axis',(0.,0.,1.));
#7866=DIRECTION('ref_axis',(1.,0.,0.));
#7867=DIRECTION('axis',(0.,0.,1.));
#7868=DIRECTION('refdir',(1.,0.,0.));
#7869=DIRECTION('center_axis',(0.,1.,0.));
#7870=DIRECTION('ref_axis',(1.,0.,0.));
#7871=DIRECTION('center_axis',(0.,1.,0.));
#7872=DIRECTION('ref_axis',(1.,0.,0.));
#7873=DIRECTION('',(0.,1.,0.));
#7874=DIRECTION('center_axis',(0.,-1.,0.));
#7875=DIRECTION('ref_axis',(1.,0.,0.));
#7876=DIRECTION('center_axis',(0.,1.,0.));
#7877=DIRECTION('ref_axis',(1.,0.,0.));
#7878=DIRECTION('center_axis',(0.,1.,0.));
#7879=DIRECTION('ref_axis',(1.,0.,0.));
#7880=DIRECTION('center_axis',(0.,1.,0.));
#7881=DIRECTION('ref_axis',(1.,0.,0.));
#7882=DIRECTION('center_axis',(0.,1.,0.));
#7883=DIRECTION('ref_axis',(1.,0.,0.));
#7884=DIRECTION('center_axis',(0.,1.,0.));
#7885=DIRECTION('ref_axis',(1.,0.,0.));
#7886=DIRECTION('',(0.,-1.,0.));
#7887=DIRECTION('center_axis',(0.,1.,0.));
#7888=DIRECTION('ref_axis',(1.,0.,0.));
#7889=DIRECTION('center_axis',(0.,1.,0.));
#7890=DIRECTION('ref_axis',(1.,0.,0.));
#7891=DIRECTION('center_axis',(0.,1.,0.));
#7892=DIRECTION('ref_axis',(1.,0.,0.));
#7893=DIRECTION('center_axis',(0.,1.,0.));
#7894=DIRECTION('ref_axis',(1.,0.,0.));
#7895=DIRECTION('',(0.,-1.,0.));
#7896=DIRECTION('center_axis',(0.,1.,0.));
#7897=DIRECTION('ref_axis',(1.,0.,0.));
#7898=DIRECTION('axis',(0.,0.,1.));
#7899=DIRECTION('refdir',(1.,0.,0.));
#7900=DIRECTION('center_axis',(0.,1.,0.));
#7901=DIRECTION('ref_axis',(1.,0.,0.));
#7902=DIRECTION('center_axis',(0.,-1.,0.));
#7903=DIRECTION('ref_axis',(1.,0.,0.));
#7904=DIRECTION('',(0.,-1.,0.));
#7905=DIRECTION('center_axis',(0.,-1.,0.));
#7906=DIRECTION('ref_axis',(1.,0.,0.));
#7907=DIRECTION('center_axis',(0.,1.,0.));
#7908=DIRECTION('ref_axis',(1.,0.,0.));
#7909=DIRECTION('center_axis',(0.,1.,0.));
#7910=DIRECTION('ref_axis',(1.,0.,0.));
#7911=DIRECTION('',(0.,-1.,0.));
#7912=DIRECTION('center_axis',(0.,1.,0.));
#7913=DIRECTION('ref_axis',(1.,0.,0.));
#7914=DIRECTION('center_axis',(0.,1.,0.));
#7915=DIRECTION('ref_axis',(1.,0.,0.));
#7916=DIRECTION('center_axis',(0.,1.,0.));
#7917=DIRECTION('ref_axis',(1.,0.,0.));
#7918=DIRECTION('axis',(0.,0.,1.));
#7919=DIRECTION('refdir',(1.,0.,0.));
#7920=DIRECTION('center_axis',(0.,1.,0.));
#7921=DIRECTION('ref_axis',(1.,0.,0.));
#7922=DIRECTION('center_axis',(0.,-1.,0.));
#7923=DIRECTION('ref_axis',(1.,0.,0.));
#7924=DIRECTION('',(0.,-1.,0.));
#7925=DIRECTION('center_axis',(0.,-1.,0.));
#7926=DIRECTION('ref_axis',(1.,0.,0.));
#7927=DIRECTION('center_axis',(0.,1.,0.));
#7928=DIRECTION('ref_axis',(1.,0.,0.));
#7929=DIRECTION('center_axis',(0.,1.,0.));
#7930=DIRECTION('ref_axis',(1.,0.,0.));
#7931=DIRECTION('',(0.,-1.,0.));
#7932=DIRECTION('center_axis',(0.,1.,0.));
#7933=DIRECTION('ref_axis',(1.,0.,0.));
#7934=DIRECTION('center_axis',(0.,1.,0.));
#7935=DIRECTION('ref_axis',(1.,0.,0.));
#7936=DIRECTION('center_axis',(0.,1.,0.));
#7937=DIRECTION('ref_axis',(1.,0.,0.));
#7938=DIRECTION('axis',(0.,0.,1.));
#7939=DIRECTION('refdir',(1.,0.,0.));
#7940=DIRECTION('center_axis',(-0.926809259863616,0.,-0.37553241648499));
#7941=DIRECTION('ref_axis',(-0.37553241648499,0.,0.926809259863616));
#7942=DIRECTION('',(0.37553241648499,0.,-0.926809259863616));
#7943=DIRECTION('',(0.,1.,0.));
#7944=DIRECTION('',(-0.37553241648499,0.,0.926809259863616));
#7945=DIRECTION('',(0.,1.,0.));
#7946=DIRECTION('center_axis',(0.,0.,-1.));
#7947=DIRECTION('ref_axis',(-1.,0.,0.));
#7948=DIRECTION('',(1.,0.,0.));
#7949=DIRECTION('',(-1.,0.,0.));
#7950=DIRECTION('',(0.,1.,0.));
#7951=DIRECTION('center_axis',(0.926809259863616,0.,0.37553241648499));
#7952=DIRECTION('ref_axis',(0.37553241648499,0.,-0.926809259863616));
#7953=DIRECTION('',(-0.37553241648499,0.,0.926809259863616));
#7954=DIRECTION('',(0.37553241648499,0.,-0.926809259863616));
#7955=DIRECTION('',(0.,1.,0.));
#7956=DIRECTION('center_axis',(0.,0.,1.));
#7957=DIRECTION('ref_axis',(1.,0.,0.));
#7958=DIRECTION('',(-1.,0.,0.));
#7959=DIRECTION('',(1.,0.,0.));
#7960=DIRECTION('center_axis',(0.,1.,0.));
#7961=DIRECTION('ref_axis',(0.,0.,1.));
#7962=DIRECTION('center_axis',(0.,1.,0.));
#7963=DIRECTION('ref_axis',(1.,0.,0.));
#7964=DIRECTION('axis',(0.,0.,1.));
#7965=DIRECTION('refdir',(1.,0.,0.));
#7966=DIRECTION('center_axis',(0.,0.,1.));
#7967=DIRECTION('ref_axis',(1.,0.,0.));
#7968=DIRECTION('center_axis',(0.,0.,1.));
#7969=DIRECTION('ref_axis',(1.,0.,0.));
#7970=DIRECTION('',(0.,0.,1.));
#7971=DIRECTION('center_axis',(0.,0.,-1.));
#7972=DIRECTION('ref_axis',(1.,0.,0.));
#7973=DIRECTION('center_axis',(0.,1.,0.));
#7974=DIRECTION('ref_axis',(-1.,0.,0.));
#7975=DIRECTION('',(-1.,0.,0.));
#7976=DIRECTION('',(0.,0.,1.));
#7977=DIRECTION('',(-1.,0.,0.));
#7978=DIRECTION('',(0.,0.,1.));
#7979=DIRECTION('center_axis',(1.,0.,0.));
#7980=DIRECTION('ref_axis',(0.,1.,0.));
#7981=DIRECTION('',(0.,1.,0.));
#7982=DIRECTION('',(0.,1.,0.));
#7983=DIRECTION('',(0.,0.,1.));
#7984=DIRECTION('center_axis',(0.,-1.,0.));
#7985=DIRECTION('ref_axis',(1.,0.,0.));
#7986=DIRECTION('',(1.,0.,0.));
#7987=DIRECTION('',(1.,0.,0.));
#7988=DIRECTION('',(0.,0.,1.));
#7989=DIRECTION('center_axis',(-1.,0.,0.));
#7990=DIRECTION('ref_axis',(0.,-1.,0.));
#7991=DIRECTION('',(0.,-1.,0.));
#7992=DIRECTION('',(0.,-1.,0.));
#7993=DIRECTION('center_axis',(0.,0.,1.));
#7994=DIRECTION('ref_axis',(1.,0.,0.));
#7995=DIRECTION('center_axis',(0.,0.,1.));
#7996=DIRECTION('ref_axis',(1.,0.,0.));
#7997=DIRECTION('axis',(0.,0.,1.));
#7998=DIRECTION('refdir',(1.,0.,0.));
#7999=DIRECTION('axis',(0.,0.,1.));
#8000=DIRECTION('refdir',(1.,0.,0.));
#8001=DIRECTION('center_axis',(0.,1.,0.));
#8002=DIRECTION('ref_axis',(1.,0.,0.));
#8003=DIRECTION('center_axis',(0.,1.,0.));
#8004=DIRECTION('ref_axis',(1.,0.,0.));
#8005=DIRECTION('',(0.,1.,0.));
#8006=DIRECTION('center_axis',(0.,-1.,0.));
#8007=DIRECTION('ref_axis',(1.,0.,0.));
#8008=DIRECTION('center_axis',(0.,1.,0.));
#8009=DIRECTION('ref_axis',(1.,0.,0.));
#8010=DIRECTION('center_axis',(0.,1.,0.));
#8011=DIRECTION('ref_axis',(1.,0.,0.));
#8012=DIRECTION('',(0.,1.,0.));
#8013=DIRECTION('center_axis',(0.,-1.,0.));
#8014=DIRECTION('ref_axis',(1.,0.,0.));
#8015=DIRECTION('center_axis',(6.12323399573677E-17,0.,1.));
#8016=DIRECTION('ref_axis',(1.,0.,0.));
#8017=DIRECTION('center_axis',(-1.22464679914735E-16,1.,0.));
#8018=DIRECTION('ref_axis',(-1.,-1.22464679914735E-16,0.));
#8019=DIRECTION('center_axis',(0.,1.,0.));
#8020=DIRECTION('ref_axis',(0.,0.,1.));
#8021=DIRECTION('',(1.,0.,0.));
#8022=DIRECTION('',(0.850265146687862,0.,0.526354614616295));
#8023=DIRECTION('center_axis',(0.,1.,0.));
#8024=DIRECTION('ref_axis',(1.,0.,0.));
#8025=DIRECTION('center_axis',(0.,1.,0.));
#8026=DIRECTION('ref_axis',(0.,0.,1.));
#8027=DIRECTION('',(1.,0.,0.));
#8028=DIRECTION('center_axis',(0.,1.,0.));
#8029=DIRECTION('ref_axis',(1.,0.,0.));
#8030=DIRECTION('',(0.850265146687862,0.,-0.526354614616295));
#8031=DIRECTION('center_axis',(0.,-1.,0.));
#8032=DIRECTION('ref_axis',(0.,0.,-1.));
#8033=DIRECTION('',(-1.,0.,0.));
#8034=DIRECTION('center_axis',(0.,-1.,0.));
#8035=DIRECTION('ref_axis',(1.,0.,0.));
#8036=DIRECTION('',(-0.850265146687862,0.,-0.526354614616295));
#8037=DIRECTION('center_axis',(-0.526354614616295,0.,0.850265146687862));
#8038=DIRECTION('ref_axis',(0.850265146687862,0.,0.526354614616295));
#8039=DIRECTION('',(0.,1.,0.));
#8040=DIRECTION('',(0.,-1.,0.));
#8041=DIRECTION('center_axis',(0.,-1.,0.));
#8042=DIRECTION('ref_axis',(0.,0.,-1.));
#8043=DIRECTION('',(-1.,0.,0.));
#8044=DIRECTION('',(-0.850265146687862,0.,0.526354614616295));
#8045=DIRECTION('center_axis',(0.,-1.,0.));
#8046=DIRECTION('ref_axis',(1.,0.,0.));
#8047=DIRECTION('center_axis',(0.526354614616295,0.,0.850265146687862));
#8048=DIRECTION('ref_axis',(0.850265146687862,0.,-0.526354614616295));
#8049=DIRECTION('',(0.,-1.,0.));
#8050=DIRECTION('',(0.,1.,0.));
#8051=DIRECTION('center_axis',(0.,0.,1.));
#8052=DIRECTION('ref_axis',(1.,0.,0.));
#8053=DIRECTION('',(0.,-1.,0.));
#8054=DIRECTION('',(1.,0.,0.));
#8055=DIRECTION('',(0.,1.,0.));
#8056=DIRECTION('',(-1.,0.,0.));
#8057=DIRECTION('center_axis',(0.,0.,-1.));
#8058=DIRECTION('ref_axis',(1.,0.,0.));
#8059=DIRECTION('center_axis',(0.,0.,-1.));
#8060=DIRECTION('ref_axis',(1.,0.,0.));
#8061=DIRECTION('',(0.,-1.,0.));
#8062=DIRECTION('',(-1.,0.,0.));
#8063=DIRECTION('',(0.,1.,0.));
#8064=DIRECTION('',(0.,1.,0.));
#8065=DIRECTION('',(1.,0.,0.));
#8066=DIRECTION('',(0.,-1.,0.));
#8067=DIRECTION('center_axis',(0.,1.,0.));
#8068=DIRECTION('ref_axis',(6.12323399573677E-17,0.,1.));
#8069=DIRECTION('center_axis',(0.,1.,0.));
#8070=DIRECTION('ref_axis',(1.,0.,0.));
#8071=DIRECTION('center_axis',(0.,-1.,0.));
#8072=DIRECTION('ref_axis',(1.,0.,0.));
#8073=DIRECTION('center_axis',(0.,1.,0.));
#8074=DIRECTION('ref_axis',(1.,0.,0.));
#8075=DIRECTION('center_axis',(0.,1.,0.));
#8076=DIRECTION('ref_axis',(1.,0.,0.));
#8077=DIRECTION('center_axis',(0.,1.,0.));
#8078=DIRECTION('ref_axis',(-1.,0.,0.));
#8079=DIRECTION('',(-1.,0.,0.));
#8080=DIRECTION('',(0.,0.,1.));
#8081=DIRECTION('',(-1.,0.,0.));
#8082=DIRECTION('',(0.,0.,1.));
#8083=DIRECTION('center_axis',(1.,0.,0.));
#8084=DIRECTION('ref_axis',(0.,1.,0.));
#8085=DIRECTION('',(0.,1.,0.));
#8086=DIRECTION('',(0.,0.,1.));
#8087=DIRECTION('',(0.,1.,0.));
#8088=DIRECTION('center_axis',(0.,-1.,0.));
#8089=DIRECTION('ref_axis',(1.,0.,0.));
#8090=DIRECTION('',(1.,0.,0.));
#8091=DIRECTION('',(0.,0.,1.));
#8092=DIRECTION('',(1.,0.,0.));
#8093=DIRECTION('center_axis',(-1.,0.,0.));
#8094=DIRECTION('ref_axis',(0.,-1.,0.));
#8095=DIRECTION('',(0.,-1.,0.));
#8096=DIRECTION('',(0.,-1.,0.));
#8097=DIRECTION('center_axis',(0.,0.,1.));
#8098=DIRECTION('ref_axis',(1.,0.,0.));
#8099=DIRECTION('center_axis',(0.,0.,1.));
#8100=DIRECTION('ref_axis',(1.,0.,0.));
#8101=DIRECTION('center_axis',(0.,0.,1.));
#8102=DIRECTION('ref_axis',(1.,0.,0.));
#8103=DIRECTION('',(0.,0.,1.));
#8104=DIRECTION('center_axis',(0.,0.,1.));
#8105=DIRECTION('ref_axis',(1.,0.,0.));
#8106=DIRECTION('center_axis',(0.,0.,1.));
#8107=DIRECTION('ref_axis',(1.,0.,0.));
#8108=DIRECTION('',(0.,0.,1.));
#8109=DIRECTION('center_axis',(0.,1.,0.));
#8110=DIRECTION('ref_axis',(-1.,0.,0.));
#8111=DIRECTION('',(-1.,0.,0.));
#8112=DIRECTION('',(0.,0.,1.));
#8113=DIRECTION('',(0.,0.,1.));
#8114=DIRECTION('center_axis',(1.,0.,0.));
#8115=DIRECTION('ref_axis',(0.,1.,0.));
#8116=DIRECTION('',(0.,1.,0.));
#8117=DIRECTION('',(0.,0.,1.));
#8118=DIRECTION('center_axis',(0.,-1.,0.));
#8119=DIRECTION('ref_axis',(1.,0.,0.));
#8120=DIRECTION('',(1.,0.,0.));
#8121=DIRECTION('',(0.,0.,1.));
#8122=DIRECTION('center_axis',(-1.,0.,0.));
#8123=DIRECTION('ref_axis',(0.,-1.,0.));
#8124=DIRECTION('',(0.,-1.,0.));
#8125=DIRECTION('center_axis',(0.,0.,1.));
#8126=DIRECTION('ref_axis',(1.,0.,0.));
#8127=DIRECTION('axis',(0.,0.,1.));
#8128=DIRECTION('refdir',(1.,0.,0.));
#8129=DIRECTION('center_axis',(0.,-1.,0.));
#8130=DIRECTION('ref_axis',(1.,0.,0.));
#8131=DIRECTION('center_axis',(0.,-1.,0.));
#8132=DIRECTION('ref_axis',(1.,0.,0.));
#8133=DIRECTION('',(0.,1.,0.));
#8134=DIRECTION('center_axis',(0.,-1.,0.));
#8135=DIRECTION('ref_axis',(1.,0.,0.));
#8136=DIRECTION('center_axis',(0.,1.,0.));
#8137=DIRECTION('ref_axis',(0.,0.,1.));
#8138=DIRECTION('center_axis',(0.,-1.,0.));
#8139=DIRECTION('ref_axis',(1.,0.,0.));
#8140=DIRECTION('center_axis',(6.12323399573677E-17,0.,1.));
#8141=DIRECTION('ref_axis',(1.,0.,0.));
#8142=DIRECTION('center_axis',(1.22464679914735E-16,-1.,0.));
#8143=DIRECTION('ref_axis',(-1.,-1.22464679914735E-16,0.));
#8144=DIRECTION('center_axis',(0.,-1.,0.));
#8145=DIRECTION('ref_axis',(1.,0.,0.));
#8146=DIRECTION('center_axis',(0.,-1.,0.));
#8147=DIRECTION('ref_axis',(0.,0.,-1.));
#8148=DIRECTION('center_axis',(-0.866025403784438,0.,-0.5));
#8149=DIRECTION('ref_axis',(-0.5,0.,0.866025403784438));
#8150=DIRECTION('',(-0.866025403784438,0.,-0.5));
#8151=DIRECTION('center_axis',(-0.866025403784438,0.,-0.5));
#8152=DIRECTION('ref_axis',(-0.5,0.,0.866025403784438));
#8153=DIRECTION('',(-0.866025403784438,0.,-0.5));
#8154=DIRECTION('center_axis',(0.,-1.,0.));
#8155=DIRECTION('ref_axis',(1.,0.,0.));
#8156=DIRECTION('center_axis',(0.,-1.,0.));
#8157=DIRECTION('ref_axis',(1.,0.,0.));
#8158=DIRECTION('',(0.,1.,0.));
#8159=DIRECTION('center_axis',(0.,-1.,0.));
#8160=DIRECTION('ref_axis',(1.,0.,0.));
#8161=DIRECTION('center_axis',(0.866025403784439,0.,-0.5));
#8162=DIRECTION('ref_axis',(-0.5,0.,-0.866025403784439));
#8163=DIRECTION('',(0.866025403784439,0.,-0.5));
#8164=DIRECTION('center_axis',(0.866025403784439,0.,-0.5));
#8165=DIRECTION('ref_axis',(-0.5,0.,-0.866025403784439));
#8166=DIRECTION('',(0.866025403784439,0.,-0.5));
#8167=DIRECTION('center_axis',(0.,0.,1.));
#8168=DIRECTION('ref_axis',(1.,0.,0.));
#8169=DIRECTION('',(0.,0.,1.));
#8170=DIRECTION('center_axis',(0.,0.,1.));
#8171=DIRECTION('ref_axis',(1.,0.,0.));
#8172=DIRECTION('',(0.,0.,1.));
#8173=DIRECTION('center_axis',(0.,1.,0.));
#8174=DIRECTION('ref_axis',(0.,0.,1.));
#8175=DIRECTION('center_axis',(0.,-1.,0.));
#8176=DIRECTION('ref_axis',(1.,0.,0.));
#8177=DIRECTION('center_axis',(0.,1.,0.));
#8178=DIRECTION('ref_axis',(0.,0.,1.));
#8179=DIRECTION('center_axis',(0.,-1.,0.));
#8180=DIRECTION('ref_axis',(1.,0.,0.));
#8181=DIRECTION('center_axis',(0.,-1.,0.));
#8182=DIRECTION('ref_axis',(1.,0.,0.));
#8183=DIRECTION('center_axis',(0.,-1.,0.));
#8184=DIRECTION('ref_axis',(1.,0.,0.));
#8185=DIRECTION('',(0.,1.,0.));
#8186=DIRECTION('center_axis',(0.,-1.,0.));
#8187=DIRECTION('ref_axis',(0.,0.,-1.));
#8188=DIRECTION('center_axis',(0.,-1.,0.));
#8189=DIRECTION('ref_axis',(1.,0.,0.));
#8190=DIRECTION('center_axis',(0.,-1.,0.));
#8191=DIRECTION('ref_axis',(1.,0.,0.));
#8192=DIRECTION('',(0.,1.,0.));
#8193=DIRECTION('',(0.,0.,1.));
#8194=DIRECTION('',(1.,0.,0.));
#8195=DIRECTION('',(0.,0.,1.));
#8196=DIRECTION('',(1.,0.,0.));
#8197=DIRECTION('axis',(0.,0.,1.));
#8198=DIRECTION('refdir',(1.,0.,0.));
#8199=DIRECTION('center_axis',(0.,1.,0.));
#8200=DIRECTION('ref_axis',(1.,0.,0.));
#8201=DIRECTION('center_axis',(0.,-1.,0.));
#8202=DIRECTION('ref_axis',(1.,0.,0.));
#8203=DIRECTION('',(0.,-1.,0.));
#8204=DIRECTION('center_axis',(0.,-1.,0.));
#8205=DIRECTION('ref_axis',(1.,0.,0.));
#8206=DIRECTION('center_axis',(0.,1.,0.));
#8207=DIRECTION('ref_axis',(1.,0.,0.));
#8208=DIRECTION('center_axis',(0.,1.,0.));
#8209=DIRECTION('ref_axis',(1.,0.,0.));
#8210=DIRECTION('',(0.,-1.,0.));
#8211=DIRECTION('center_axis',(0.,1.,0.));
#8212=DIRECTION('ref_axis',(1.,0.,0.));
#8213=DIRECTION('center_axis',(0.,1.,0.));
#8214=DIRECTION('ref_axis',(1.,0.,0.));
#8215=DIRECTION('center_axis',(0.,1.,0.));
#8216=DIRECTION('ref_axis',(1.,0.,0.));
#8217=DIRECTION('axis',(0.,0.,1.));
#8218=DIRECTION('refdir',(1.,0.,0.));
#8219=DIRECTION('center_axis',(0.866025403784439,0.,-0.5));
#8220=DIRECTION('ref_axis',(0.5,0.,0.866025403784439));
#8221=DIRECTION('',(-0.5,0.,-0.866025403784439));
#8222=DIRECTION('',(0.,-1.,0.));
#8223=DIRECTION('',(0.5,0.,0.866025403784439));
#8224=DIRECTION('',(0.,-1.,0.));
#8225=DIRECTION('center_axis',(1.60246890531964E-16,0.,-1.));
#8226=DIRECTION('ref_axis',(1.,0.,1.60246890531964E-16));
#8227=DIRECTION('',(-1.,0.,-1.60246890531964E-16));
#8228=DIRECTION('',(0.,-1.,0.));
#8229=DIRECTION('',(1.,0.,1.60246890531964E-16));
#8230=DIRECTION('center_axis',(-0.866025403784439,0.,-0.5));
#8231=DIRECTION('ref_axis',(0.5,0.,-0.866025403784439));
#8232=DIRECTION('',(-0.5,0.,0.866025403784439));
#8233=DIRECTION('',(0.,-1.,0.));
#8234=DIRECTION('',(0.5,0.,-0.866025403784439));
#8235=DIRECTION('center_axis',(-0.866025403784439,0.,0.5));
#8236=DIRECTION('ref_axis',(-0.5,0.,-0.866025403784439));
#8237=DIRECTION('',(0.5,0.,0.866025403784439));
#8238=DIRECTION('',(0.,-1.,0.));
#8239=DIRECTION('',(-0.5,0.,-0.866025403784439));
#8240=DIRECTION('center_axis',(-1.60246890531964E-16,0.,1.));
#8241=DIRECTION('ref_axis',(-1.,0.,-1.60246890531964E-16));
#8242=DIRECTION('',(1.,0.,1.60246890531964E-16));
#8243=DIRECTION('',(0.,-1.,0.));
#8244=DIRECTION('',(-1.,0.,-1.60246890531964E-16));
#8245=DIRECTION('center_axis',(0.866025403784439,0.,0.5));
#8246=DIRECTION('ref_axis',(-0.5,0.,0.866025403784439));
#8247=DIRECTION('',(0.5,0.,-0.866025403784439));
#8248=DIRECTION('',(-0.5,0.,0.866025403784439));
#8249=DIRECTION('center_axis',(0.,1.,0.));
#8250=DIRECTION('ref_axis',(1.,0.,0.));
#8251=DIRECTION('center_axis',(0.,-1.,0.));
#8252=DIRECTION('ref_axis',(0.,0.,-1.));
#8253=DIRECTION('center_axis',(0.,1.,0.));
#8254=DIRECTION('ref_axis',(1.,0.,0.));
#8255=DIRECTION('center_axis',(0.,1.,0.));
#8256=DIRECTION('ref_axis',(1.,0.,0.));
#8257=DIRECTION('center_axis',(0.,1.,0.));
#8258=DIRECTION('ref_axis',(0.,0.,1.));
#8259=DIRECTION('center_axis',(0.,-1.,0.));
#8260=DIRECTION('ref_axis',(1.,0.,0.));
#8261=DIRECTION('center_axis',(0.,-1.,0.));
#8262=DIRECTION('ref_axis',(1.,0.,0.));
#8263=DIRECTION('center_axis',(0.,-1.,0.));
#8264=DIRECTION('ref_axis',(1.,0.,0.));
#8265=DIRECTION('',(0.707106781186548,0.707106781186547,8.65956056235493E-17));
#8266=DIRECTION('center_axis',(0.,-1.,0.));
#8267=DIRECTION('ref_axis',(1.,0.,0.));
#8268=DIRECTION('center_axis',(0.,-1.,0.));
#8269=DIRECTION('ref_axis',(1.,0.,0.));
#8270=DIRECTION('',(0.,1.,0.));
#8271=DIRECTION('center_axis',(0.,1.,0.));
#8272=DIRECTION('ref_axis',(1.,0.,0.));
#8273=DIRECTION('center_axis',(0.,-1.,0.));
#8274=DIRECTION('ref_axis',(1.,0.,0.));
#8275=DIRECTION('',(-0.707106781186548,0.707106781186547,-8.65956056235494E-17));
#8276=DIRECTION('center_axis',(0.,-1.,0.));
#8277=DIRECTION('ref_axis',(0.,0.,-1.));
#8278=DIRECTION('center_axis',(0.,-1.,0.));
#8279=DIRECTION('ref_axis',(1.,0.,0.));
#8280=DIRECTION('center_axis',(0.,1.,0.));
#8281=DIRECTION('ref_axis',(1.,0.,0.));
#8282=DIRECTION('center_axis',(0.,1.,0.));
#8283=DIRECTION('ref_axis',(1.,0.,0.));
#8284=DIRECTION('',(-0.447213595499958,0.894427190999916,-5.47678698264203E-17));
#8285=DIRECTION('center_axis',(0.,-1.,0.));
#8286=DIRECTION('ref_axis',(1.,0.,0.));
#8287=DIRECTION('',(0.,1.,0.));
#8288=DIRECTION('axis',(0.,0.,1.));
#8289=DIRECTION('refdir',(1.,0.,0.));
#8290=DIRECTION('center_axis',(0.866025403784439,0.,-0.5));
#8291=DIRECTION('ref_axis',(0.5,0.,0.866025403784439));
#8292=DIRECTION('',(-0.5,0.,-0.866025403784439));
#8293=DIRECTION('',(0.,-1.,0.));
#8294=DIRECTION('',(0.5,0.,0.866025403784439));
#8295=DIRECTION('',(0.,-1.,0.));
#8296=DIRECTION('center_axis',(1.60246890531964E-16,0.,-1.));
#8297=DIRECTION('ref_axis',(1.,0.,1.60246890531964E-16));
#8298=DIRECTION('',(-1.,0.,-1.60246890531964E-16));
#8299=DIRECTION('',(0.,-1.,0.));
#8300=DIRECTION('',(1.,0.,1.60246890531964E-16));
#8301=DIRECTION('center_axis',(-0.866025403784439,0.,-0.5));
#8302=DIRECTION('ref_axis',(0.5,0.,-0.866025403784439));
#8303=DIRECTION('',(-0.5,0.,0.866025403784439));
#8304=DIRECTION('',(0.,-1.,0.));
#8305=DIRECTION('',(0.5,0.,-0.866025403784439));
#8306=DIRECTION('center_axis',(-0.866025403784439,0.,0.5));
#8307=DIRECTION('ref_axis',(-0.5,0.,-0.866025403784439));
#8308=DIRECTION('',(0.5,0.,0.866025403784439));
#8309=DIRECTION('',(0.,-1.,0.));
#8310=DIRECTION('',(-0.5,0.,-0.866025403784439));
#8311=DIRECTION('center_axis',(-1.60246890531964E-16,0.,1.));
#8312=DIRECTION('ref_axis',(-1.,0.,-1.60246890531964E-16));
#8313=DIRECTION('',(1.,0.,1.60246890531964E-16));
#8314=DIRECTION('',(0.,-1.,0.));
#8315=DIRECTION('',(-1.,0.,-1.60246890531964E-16));
#8316=DIRECTION('center_axis',(0.866025403784439,0.,0.5));
#8317=DIRECTION('ref_axis',(-0.5,0.,0.866025403784439));
#8318=DIRECTION('',(0.5,0.,-0.866025403784439));
#8319=DIRECTION('',(-0.5,0.,0.866025403784439));
#8320=DIRECTION('center_axis',(0.,1.,0.));
#8321=DIRECTION('ref_axis',(1.,0.,0.));
#8322=DIRECTION('center_axis',(0.,-1.,0.));
#8323=DIRECTION('ref_axis',(0.,0.,-1.));
#8324=DIRECTION('center_axis',(0.,1.,0.));
#8325=DIRECTION('ref_axis',(1.,0.,0.));
#8326=DIRECTION('center_axis',(0.,1.,0.));
#8327=DIRECTION('ref_axis',(1.,0.,0.));
#8328=DIRECTION('center_axis',(0.,1.,0.));
#8329=DIRECTION('ref_axis',(0.,0.,1.));
#8330=DIRECTION('center_axis',(0.,-1.,0.));
#8331=DIRECTION('ref_axis',(1.,0.,0.));
#8332=DIRECTION('center_axis',(0.,-1.,0.));
#8333=DIRECTION('ref_axis',(1.,0.,0.));
#8334=DIRECTION('center_axis',(0.,-1.,0.));
#8335=DIRECTION('ref_axis',(1.,0.,0.));
#8336=DIRECTION('',(0.707106781186547,0.707106781186548,8.65956056235493E-17));
#8337=DIRECTION('center_axis',(0.,-1.,0.));
#8338=DIRECTION('ref_axis',(1.,0.,0.));
#8339=DIRECTION('center_axis',(0.,-1.,0.));
#8340=DIRECTION('ref_axis',(1.,0.,0.));
#8341=DIRECTION('',(0.,1.,0.));
#8342=DIRECTION('center_axis',(0.,1.,0.));
#8343=DIRECTION('ref_axis',(1.,0.,0.));
#8344=DIRECTION('center_axis',(0.,-1.,0.));
#8345=DIRECTION('ref_axis',(1.,0.,0.));
#8346=DIRECTION('',(-0.707106781186547,0.707106781186548,-8.65956056235493E-17));
#8347=DIRECTION('center_axis',(0.,-1.,0.));
#8348=DIRECTION('ref_axis',(0.,0.,-1.));
#8349=DIRECTION('center_axis',(0.,-1.,0.));
#8350=DIRECTION('ref_axis',(1.,0.,0.));
#8351=DIRECTION('center_axis',(0.,1.,0.));
#8352=DIRECTION('ref_axis',(1.,0.,0.));
#8353=DIRECTION('center_axis',(0.,1.,0.));
#8354=DIRECTION('ref_axis',(1.,0.,0.));
#8355=DIRECTION('',(-0.447213595499958,0.894427190999916,-5.47678698264203E-17));
#8356=DIRECTION('center_axis',(0.,-1.,0.));
#8357=DIRECTION('ref_axis',(1.,0.,0.));
#8358=DIRECTION('',(0.,1.,0.));
#8359=DIRECTION('axis',(0.,0.,1.));
#8360=DIRECTION('refdir',(1.,0.,0.));
#8361=DIRECTION('axis',(0.,0.,1.));
#8362=DIRECTION('refdir',(1.,0.,0.));
#8363=DIRECTION('center_axis',(0.,1.,0.));
#8364=DIRECTION('ref_axis',(1.,0.,0.));
#8365=DIRECTION('center_axis',(0.,1.,0.));
#8366=DIRECTION('ref_axis',(1.,0.,0.));
#8367=DIRECTION('',(0.,-1.,0.));
#8368=DIRECTION('center_axis',(0.,1.,0.));
#8369=DIRECTION('ref_axis',(1.,0.,0.));
#8370=DIRECTION('center_axis',(0.,1.,0.));
#8371=DIRECTION('ref_axis',(1.,0.,0.));
#8372=DIRECTION('center_axis',(0.,1.,0.));
#8373=DIRECTION('ref_axis',(1.,0.,0.));
#8374=DIRECTION('axis',(0.,0.,1.));
#8375=DIRECTION('refdir',(1.,0.,0.));
#8376=DIRECTION('center_axis',(0.,0.,1.));
#8377=DIRECTION('ref_axis',(1.,0.,0.));
#8378=DIRECTION('',(0.,1.,0.));
#8379=DIRECTION('center_axis',(0.,0.,1.));
#8380=DIRECTION('ref_axis',(1.,0.,0.));
#8381=DIRECTION('center_axis',(0.,0.,1.));
#8382=DIRECTION('ref_axis',(1.,0.,0.));
#8383=DIRECTION('center_axis',(0.,0.,1.));
#8384=DIRECTION('ref_axis',(1.,0.,0.));
#8385=DIRECTION('',(0.,0.,1.));
#8386=DIRECTION('center_axis',(0.,0.,1.));
#8387=DIRECTION('ref_axis',(1.,0.,0.));
#8388=DIRECTION('center_axis',(0.,0.,1.));
#8389=DIRECTION('ref_axis',(1.,0.,0.));
#8390=DIRECTION('',(0.,-1.,0.));
#8391=DIRECTION('center_axis',(0.,1.,0.));
#8392=DIRECTION('ref_axis',(1.,0.,0.));
#8393=DIRECTION('center_axis',(0.,-1.,0.));
#8394=DIRECTION('ref_axis',(1.,0.,0.));
#8395=DIRECTION('',(0.,-1.,0.));
#8396=DIRECTION('center_axis',(0.,-1.,0.));
#8397=DIRECTION('ref_axis',(1.,0.,0.));
#8398=DIRECTION('center_axis',(0.,1.,0.));
#8399=DIRECTION('ref_axis',(1.,0.,0.));
#8400=DIRECTION('center_axis',(0.,1.,0.));
#8401=DIRECTION('ref_axis',(1.,0.,0.));
#8402=DIRECTION('',(0.,-1.,0.));
#8403=DIRECTION('center_axis',(0.,1.,0.));
#8404=DIRECTION('ref_axis',(1.,0.,0.));
#8405=DIRECTION('center_axis',(0.,1.,0.));
#8406=DIRECTION('ref_axis',(1.,0.,0.));
#8407=DIRECTION('center_axis',(0.,1.,0.));
#8408=DIRECTION('ref_axis',(1.,0.,0.));
#8409=DIRECTION('axis',(0.,0.,1.));
#8410=DIRECTION('refdir',(1.,0.,0.));
#8411=DIRECTION('center_axis',(0.,0.,1.));
#8412=DIRECTION('ref_axis',(1.,0.,0.));
#8413=DIRECTION('',(0.,1.,0.));
#8414=DIRECTION('center_axis',(0.,0.,1.));
#8415=DIRECTION('ref_axis',(1.,0.,0.));
#8416=DIRECTION('center_axis',(0.,0.,1.));
#8417=DIRECTION('ref_axis',(1.,0.,0.));
#8418=DIRECTION('center_axis',(0.,0.,1.));
#8419=DIRECTION('ref_axis',(1.,0.,0.));
#8420=DIRECTION('',(0.,0.,1.));
#8421=DIRECTION('center_axis',(0.,0.,1.));
#8422=DIRECTION('ref_axis',(1.,0.,0.));
#8423=DIRECTION('center_axis',(0.,0.,1.));
#8424=DIRECTION('ref_axis',(1.,0.,0.));
#8425=DIRECTION('',(0.,-1.,0.));
#8426=DIRECTION('center_axis',(0.,1.,0.));
#8427=DIRECTION('ref_axis',(1.,0.,0.));
#8428=DIRECTION('center_axis',(0.,-1.,0.));
#8429=DIRECTION('ref_axis',(1.,0.,0.));
#8430=DIRECTION('',(0.,-1.,0.));
#8431=DIRECTION('center_axis',(0.,-1.,0.));
#8432=DIRECTION('ref_axis',(1.,0.,0.));
#8433=DIRECTION('center_axis',(0.,1.,0.));
#8434=DIRECTION('ref_axis',(1.,0.,0.));
#8435=DIRECTION('center_axis',(0.,1.,0.));
#8436=DIRECTION('ref_axis',(1.,0.,0.));
#8437=DIRECTION('',(0.,-1.,0.));
#8438=DIRECTION('center_axis',(0.,1.,0.));
#8439=DIRECTION('ref_axis',(1.,0.,0.));
#8440=DIRECTION('center_axis',(0.,1.,0.));
#8441=DIRECTION('ref_axis',(1.,0.,0.));
#8442=DIRECTION('center_axis',(0.,1.,0.));
#8443=DIRECTION('ref_axis',(1.,0.,0.));
#8444=DIRECTION('axis',(0.,0.,1.));
#8445=DIRECTION('refdir',(1.,0.,0.));
#8446=DIRECTION('center_axis',(0.,1.,0.));
#8447=DIRECTION('ref_axis',(1.,0.,0.));
#8448=DIRECTION('center_axis',(0.,-1.,0.));
#8449=DIRECTION('ref_axis',(1.,0.,0.));
#8450=DIRECTION('',(0.,-1.,0.));
#8451=DIRECTION('center_axis',(0.,-1.,0.));
#8452=DIRECTION('ref_axis',(1.,0.,0.));
#8453=DIRECTION('center_axis',(0.,1.,0.));
#8454=DIRECTION('ref_axis',(1.,0.,0.));
#8455=DIRECTION('center_axis',(0.,1.,0.));
#8456=DIRECTION('ref_axis',(1.,0.,0.));
#8457=DIRECTION('',(0.,-1.,0.));
#8458=DIRECTION('center_axis',(0.,1.,0.));
#8459=DIRECTION('ref_axis',(1.,0.,0.));
#8460=DIRECTION('center_axis',(0.,1.,0.));
#8461=DIRECTION('ref_axis',(1.,0.,0.));
#8462=DIRECTION('center_axis',(0.,1.,0.));
#8463=DIRECTION('ref_axis',(1.,0.,0.));
#8464=DIRECTION('axis',(0.,0.,1.));
#8465=DIRECTION('refdir',(1.,0.,0.));
#8466=DIRECTION('center_axis',(0.,1.,0.));
#8467=DIRECTION('ref_axis',(1.,0.,0.));
#8468=DIRECTION('center_axis',(0.,-1.,0.));
#8469=DIRECTION('ref_axis',(1.,0.,0.));
#8470=DIRECTION('',(0.,-1.,0.));
#8471=DIRECTION('center_axis',(0.,-1.,0.));
#8472=DIRECTION('ref_axis',(1.,0.,0.));
#8473=DIRECTION('center_axis',(0.,1.,0.));
#8474=DIRECTION('ref_axis',(1.,0.,0.));
#8475=DIRECTION('center_axis',(0.,1.,0.));
#8476=DIRECTION('ref_axis',(1.,0.,0.));
#8477=DIRECTION('',(0.,-1.,0.));
#8478=DIRECTION('center_axis',(0.,1.,0.));
#8479=DIRECTION('ref_axis',(1.,0.,0.));
#8480=DIRECTION('center_axis',(0.,1.,0.));
#8481=DIRECTION('ref_axis',(1.,0.,0.));
#8482=DIRECTION('center_axis',(0.,1.,0.));
#8483=DIRECTION('ref_axis',(1.,0.,0.));
#8484=DIRECTION('axis',(0.,0.,1.));
#8485=DIRECTION('refdir',(1.,0.,0.));
#8486=DIRECTION('center_axis',(0.,0.,1.));
#8487=DIRECTION('ref_axis',(1.,0.,0.));
#8488=DIRECTION('',(0.,1.,0.));
#8489=DIRECTION('center_axis',(0.,0.,1.));
#8490=DIRECTION('ref_axis',(1.,0.,0.));
#8491=DIRECTION('center_axis',(0.,0.,1.));
#8492=DIRECTION('ref_axis',(1.,0.,0.));
#8493=DIRECTION('center_axis',(0.,0.,1.));
#8494=DIRECTION('ref_axis',(1.,0.,0.));
#8495=DIRECTION('',(0.,0.,1.));
#8496=DIRECTION('center_axis',(0.,0.,1.));
#8497=DIRECTION('ref_axis',(1.,0.,0.));
#8498=DIRECTION('center_axis',(0.,0.,1.));
#8499=DIRECTION('ref_axis',(1.,0.,0.));
#8500=DIRECTION('',(0.,-1.,0.));
#8501=DIRECTION('center_axis',(0.,1.,0.));
#8502=DIRECTION('ref_axis',(1.,0.,0.));
#8503=DIRECTION('center_axis',(0.,-1.,0.));
#8504=DIRECTION('ref_axis',(1.,0.,0.));
#8505=DIRECTION('',(0.,-1.,0.));
#8506=DIRECTION('center_axis',(0.,-1.,0.));
#8507=DIRECTION('ref_axis',(1.,0.,0.));
#8508=DIRECTION('center_axis',(0.,1.,0.));
#8509=DIRECTION('ref_axis',(1.,0.,0.));
#8510=DIRECTION('center_axis',(0.,1.,0.));
#8511=DIRECTION('ref_axis',(1.,0.,0.));
#8512=DIRECTION('',(0.,-1.,0.));
#8513=DIRECTION('center_axis',(0.,1.,0.));
#8514=DIRECTION('ref_axis',(1.,0.,0.));
#8515=DIRECTION('center_axis',(0.,1.,0.));
#8516=DIRECTION('ref_axis',(1.,0.,0.));
#8517=DIRECTION('center_axis',(0.,1.,0.));
#8518=DIRECTION('ref_axis',(1.,0.,0.));
#8519=DIRECTION('axis',(0.,0.,1.));
#8520=DIRECTION('refdir',(1.,0.,0.));
#8521=DIRECTION('center_axis',(0.,1.,0.));
#8522=DIRECTION('ref_axis',(1.,0.,0.));
#8523=DIRECTION('center_axis',(0.,-1.,0.));
#8524=DIRECTION('ref_axis',(1.,0.,0.));
#8525=DIRECTION('',(0.,-1.,0.));
#8526=DIRECTION('center_axis',(0.,-1.,0.));
#8527=DIRECTION('ref_axis',(1.,0.,0.));
#8528=DIRECTION('center_axis',(0.,1.,0.));
#8529=DIRECTION('ref_axis',(1.,0.,0.));
#8530=DIRECTION('center_axis',(0.,1.,0.));
#8531=DIRECTION('ref_axis',(1.,0.,0.));
#8532=DIRECTION('',(0.,-1.,0.));
#8533=DIRECTION('center_axis',(0.,1.,0.));
#8534=DIRECTION('ref_axis',(1.,0.,0.));
#8535=DIRECTION('center_axis',(0.,1.,0.));
#8536=DIRECTION('ref_axis',(1.,0.,0.));
#8537=DIRECTION('center_axis',(0.,1.,0.));
#8538=DIRECTION('ref_axis',(1.,0.,0.));
#8539=DIRECTION('axis',(0.,0.,1.));
#8540=DIRECTION('refdir',(1.,0.,0.));
#8541=DIRECTION('center_axis',(0.,0.,1.));
#8542=DIRECTION('ref_axis',(1.,0.,0.));
#8543=DIRECTION('',(0.,1.,0.));
#8544=DIRECTION('center_axis',(0.,0.,1.));
#8545=DIRECTION('ref_axis',(1.,0.,0.));
#8546=DIRECTION('center_axis',(0.,0.,1.));
#8547=DIRECTION('ref_axis',(1.,0.,0.));
#8548=DIRECTION('center_axis',(0.,0.,1.));
#8549=DIRECTION('ref_axis',(1.,0.,0.));
#8550=DIRECTION('',(0.,0.,1.));
#8551=DIRECTION('center_axis',(0.,0.,1.));
#8552=DIRECTION('ref_axis',(1.,0.,0.));
#8553=DIRECTION('center_axis',(0.,0.,1.));
#8554=DIRECTION('ref_axis',(1.,0.,0.));
#8555=DIRECTION('',(0.,-1.,0.));
#8556=DIRECTION('center_axis',(0.,1.,0.));
#8557=DIRECTION('ref_axis',(1.,0.,0.));
#8558=DIRECTION('center_axis',(0.,-1.,0.));
#8559=DIRECTION('ref_axis',(1.,0.,0.));
#8560=DIRECTION('',(0.,-1.,0.));
#8561=DIRECTION('center_axis',(0.,-1.,0.));
#8562=DIRECTION('ref_axis',(1.,0.,0.));
#8563=DIRECTION('center_axis',(0.,1.,0.));
#8564=DIRECTION('ref_axis',(1.,0.,0.));
#8565=DIRECTION('center_axis',(0.,1.,0.));
#8566=DIRECTION('ref_axis',(1.,0.,0.));
#8567=DIRECTION('',(0.,-1.,0.));
#8568=DIRECTION('center_axis',(0.,1.,0.));
#8569=DIRECTION('ref_axis',(1.,0.,0.));
#8570=DIRECTION('center_axis',(0.,1.,0.));
#8571=DIRECTION('ref_axis',(1.,0.,0.));
#8572=DIRECTION('center_axis',(0.,1.,0.));
#8573=DIRECTION('ref_axis',(1.,0.,0.));
#8574=DIRECTION('axis',(0.,0.,1.));
#8575=DIRECTION('refdir',(1.,0.,0.));
#8576=DIRECTION('center_axis',(0.,0.,1.));
#8577=DIRECTION('ref_axis',(1.,0.,0.));
#8578=DIRECTION('',(0.,1.,0.));
#8579=DIRECTION('center_axis',(0.,0.,1.));
#8580=DIRECTION('ref_axis',(1.,0.,0.));
#8581=DIRECTION('center_axis',(0.,0.,1.));
#8582=DIRECTION('ref_axis',(1.,0.,0.));
#8583=DIRECTION('center_axis',(0.,0.,1.));
#8584=DIRECTION('ref_axis',(1.,0.,0.));
#8585=DIRECTION('',(0.,0.,1.));
#8586=DIRECTION('center_axis',(0.,0.,1.));
#8587=DIRECTION('ref_axis',(1.,0.,0.));
#8588=DIRECTION('center_axis',(0.,0.,1.));
#8589=DIRECTION('ref_axis',(1.,0.,0.));
#8590=DIRECTION('',(0.,-1.,0.));
#8591=DIRECTION('center_axis',(0.,1.,0.));
#8592=DIRECTION('ref_axis',(1.,0.,0.));
#8593=DIRECTION('center_axis',(0.,1.,0.));
#8594=DIRECTION('ref_axis',(1.,0.,0.));
#8595=DIRECTION('',(0.,-1.,0.));
#8596=DIRECTION('center_axis',(0.,-1.,0.));
#8597=DIRECTION('ref_axis',(1.,0.,0.));
#8598=DIRECTION('center_axis',(0.,1.,0.));
#8599=DIRECTION('ref_axis',(1.,0.,0.));
#8600=DIRECTION('center_axis',(0.,-1.,0.));
#8601=DIRECTION('ref_axis',(1.,0.,0.));
#8602=DIRECTION('center_axis',(0.,1.,0.));
#8603=DIRECTION('ref_axis',(1.,0.,0.));
#8604=DIRECTION('center_axis',(0.,1.,0.));
#8605=DIRECTION('ref_axis',(1.,0.,0.));
#8606=DIRECTION('',(0.,1.,0.));
#8607=DIRECTION('center_axis',(0.015706233006771,0.,0.999876649514697));
#8608=DIRECTION('ref_axis',(0.999876649514697,0.,-0.015706233006771));
#8609=DIRECTION('',(-0.999876649514697,0.,0.015706233006771));
#8610=DIRECTION('',(0.,1.,0.));
#8611=DIRECTION('',(0.999876649514697,0.,-0.015706233006771));
#8612=DIRECTION('',(0.,1.,0.));
#8613=DIRECTION('center_axis',(0.957469564385932,0.,-0.288534284400681));
#8614=DIRECTION('ref_axis',(-0.288534284400681,0.,-0.957469564385932));
#8615=DIRECTION('',(0.288534284400681,0.,0.957469564385932));
#8616=DIRECTION('',(-0.288534284400681,0.,-0.957469564385932));
#8617=DIRECTION('',(0.,1.,0.));
#8618=DIRECTION('center_axis',(-0.243616063552747,0.,0.9698717510986));
#8619=DIRECTION('ref_axis',(0.9698717510986,0.,0.243616063552747));
#8620=DIRECTION('',(-0.9698717510986,0.,-0.243616063552747));
#8621=DIRECTION('',(0.9698717510986,0.,0.243616063552747));
#8622=DIRECTION('',(0.,1.,0.));
#8623=DIRECTION('center_axis',(0.999522748094039,0.,-0.0308913587033594));
#8624=DIRECTION('ref_axis',(-0.0308913587033594,0.,-0.999522748094039));
#8625=DIRECTION('',(0.0308913587033594,0.,0.999522748094039));
#8626=DIRECTION('',(-0.0308913587033594,0.,-0.999522748094039));
#8627=DIRECTION('',(0.,1.,0.));
#8628=DIRECTION('center_axis',(-0.486336327975727,0.,0.873771695633983));
#8629=DIRECTION('ref_axis',(0.873771695633983,0.,0.486336327975727));
#8630=DIRECTION('',(-0.873771695633983,0.,-0.486336327975727));
#8631=DIRECTION('',(0.873771695633983,0.,0.486336327975727));
#8632=DIRECTION('',(0.,1.,0.));
#8633=DIRECTION('center_axis',(0.973460108308978,0.,0.228856762039213));
#8634=DIRECTION('ref_axis',(0.228856762039213,0.,-0.973460108308978));
#8635=DIRECTION('',(-0.228856762039213,0.,0.973460108308978));
#8636=DIRECTION('',(0.228856762039213,0.,-0.973460108308978));
#8637=DIRECTION('',(0.,1.,0.));
#8638=DIRECTION('center_axis',(-0.695913575355945,0.,0.71812554308791));
#8639=DIRECTION('ref_axis',(0.71812554308791,0.,0.695913575355945));
#8640=DIRECTION('',(-0.71812554308791,0.,-0.695913575355945));
#8641=DIRECTION('',(0.71812554308791,0.,0.695913575355945));
#8642=DIRECTION('',(0.,1.,0.));
#8643=DIRECTION('center_axis',(0.881057770861552,0.,0.473008672652493));
#8644=DIRECTION('ref_axis',(0.473008672652493,0.,-0.881057770861552));
#8645=DIRECTION('',(-0.473008672652493,0.,0.881057770861552));
#8646=DIRECTION('',(0.473008672652493,0.,-0.881057770861552));
#8647=DIRECTION('',(0.,1.,0.));
#8648=DIRECTION('center_axis',(-0.858065462627213,0.,0.513540321538968));
#8649=DIRECTION('ref_axis',(0.513540321538968,0.,0.858065462627213));
#8650=DIRECTION('',(-0.513540321538968,0.,-0.858065462627213));
#8651=DIRECTION('',(0.513540321538968,0.,0.858065462627213));
#8652=DIRECTION('',(0.,1.,0.));
#8653=DIRECTION('center_axis',(0.728612802346719,0.,0.684925823908298));
#8654=DIRECTION('ref_axis',(0.684925823908298,0.,-0.728612802346719));
#8655=DIRECTION('',(-0.684925823908298,0.,0.728612802346719));
#8656=DIRECTION('',(0.684925823908298,0.,-0.728612802346719));
#8657=DIRECTION('',(0.,1.,0.));
#8658=DIRECTION('center_axis',(-0.96174160664066,0.,0.273958175742654));
#8659=DIRECTION('ref_axis',(0.273958175742654,0.,0.96174160664066));
#8660=DIRECTION('',(-0.273958175742654,0.,-0.96174160664066));
#8661=DIRECTION('',(0.273958175742654,0.,0.96174160664066));
#8662=DIRECTION('',(0.,1.,0.));
#8663=DIRECTION('center_axis',(0.526514075441545,0.,0.850166412158193));
#8664=DIRECTION('ref_axis',(0.850166412158193,0.,-0.526514075441545));
#8665=DIRECTION('',(-0.850166412158193,0.,0.526514075441545));
#8666=DIRECTION('',(0.850166412158193,0.,-0.526514075441545));
#8667=DIRECTION('',(0.,1.,0.));
#8668=DIRECTION('center_axis',(-0.999876649514698,0.,0.0157062330067685));
#8669=DIRECTION('ref_axis',(0.0157062330067685,0.,0.999876649514698));
#8670=DIRECTION('',(-0.0157062330067685,0.,-0.999876649514698));
#8671=DIRECTION('',(0.0157062330067685,0.,0.999876649514698));
#8672=DIRECTION('',(0.,1.,0.));
#8673=DIRECTION('center_axis',(0.288534284400681,0.,0.957469564385932));
#8674=DIRECTION('ref_axis',(0.957469564385932,0.,-0.288534284400681));
#8675=DIRECTION('',(-0.957469564385932,0.,0.288534284400681));
#8676=DIRECTION('',(0.957469564385932,0.,-0.288534284400681));
#8677=DIRECTION('',(0.,1.,0.));
#8678=DIRECTION('center_axis',(-0.969871751098599,0.,-0.243616063552749));
#8679=DIRECTION('ref_axis',(-0.243616063552749,0.,0.969871751098599));
#8680=DIRECTION('',(0.243616063552749,0.,-0.969871751098599));
#8681=DIRECTION('',(-0.243616063552749,0.,0.969871751098599));
#8682=DIRECTION('',(0.,1.,0.));
#8683=DIRECTION('center_axis',(0.0308913587033598,0.,0.999522748094039));
#8684=DIRECTION('ref_axis',(0.999522748094039,0.,-0.0308913587033598));
#8685=DIRECTION('',(-0.999522748094039,0.,0.0308913587033598));
#8686=DIRECTION('',(0.999522748094039,0.,-0.0308913587033598));
#8687=DIRECTION('',(0.,1.,0.));
#8688=DIRECTION('center_axis',(-0.873771695633983,0.,-0.486336327975728));
#8689=DIRECTION('ref_axis',(-0.486336327975728,0.,0.873771695633983));
#8690=DIRECTION('',(0.486336327975728,0.,-0.873771695633983));
#8691=DIRECTION('',(-0.486336327975728,0.,0.873771695633983));
#8692=DIRECTION('',(0.,1.,0.));
#8693=DIRECTION('center_axis',(-0.228856762039212,0.,0.973460108308978));
#8694=DIRECTION('ref_axis',(0.973460108308978,0.,0.228856762039212));
#8695=DIRECTION('',(-0.973460108308978,0.,-0.228856762039212));
#8696=DIRECTION('',(0.973460108308978,0.,0.228856762039212));
#8697=DIRECTION('',(0.,1.,0.));
#8698=DIRECTION('center_axis',(-0.718125543087911,0.,-0.695913575355944));
#8699=DIRECTION('ref_axis',(-0.695913575355944,0.,0.718125543087911));
#8700=DIRECTION('',(0.695913575355944,0.,-0.718125543087911));
#8701=DIRECTION('',(-0.695913575355944,0.,0.718125543087911));
#8702=DIRECTION('',(0.,1.,0.));
#8703=DIRECTION('center_axis',(-0.473008672652494,0.,0.881057770861551));
#8704=DIRECTION('ref_axis',(0.881057770861551,0.,0.473008672652494));
#8705=DIRECTION('',(-0.881057770861551,0.,-0.473008672652494));
#8706=DIRECTION('',(0.881057770861551,0.,0.473008672652494));
#8707=DIRECTION('',(0.,1.,0.));
#8708=DIRECTION('center_axis',(-0.513540321538967,0.,-0.858065462627214));
#8709=DIRECTION('ref_axis',(-0.858065462627214,0.,0.513540321538967));
#8710=DIRECTION('',(0.858065462627214,0.,-0.513540321538967));
#8711=DIRECTION('',(-0.858065462627214,0.,0.513540321538967));
#8712=DIRECTION('',(0.,1.,0.));
#8713=DIRECTION('center_axis',(-0.684925823908296,0.,0.728612802346721));
#8714=DIRECTION('ref_axis',(0.728612802346721,0.,0.684925823908296));
#8715=DIRECTION('',(-0.728612802346721,0.,-0.684925823908296));
#8716=DIRECTION('',(0.728612802346721,0.,0.684925823908296));
#8717=DIRECTION('',(0.,1.,0.));
#8718=DIRECTION('center_axis',(-0.273958175742656,0.,-0.961741606640659));
#8719=DIRECTION('ref_axis',(-0.961741606640659,0.,0.273958175742656));
#8720=DIRECTION('',(0.961741606640659,0.,-0.273958175742656));
#8721=DIRECTION('',(-0.961741606640659,0.,0.273958175742656));
#8722=DIRECTION('',(0.,1.,0.));
#8723=DIRECTION('center_axis',(-0.850166412158193,0.,0.526514075441546));
#8724=DIRECTION('ref_axis',(0.526514075441546,0.,0.850166412158193));
#8725=DIRECTION('',(-0.526514075441546,0.,-0.850166412158193));
#8726=DIRECTION('',(0.526514075441546,0.,0.850166412158193));
#8727=DIRECTION('',(0.,1.,0.));
#8728=DIRECTION('center_axis',(-0.0157062330067692,0.,-0.999876649514697));
#8729=DIRECTION('ref_axis',(-0.999876649514697,0.,0.0157062330067692));
#8730=DIRECTION('',(0.999876649514697,0.,-0.0157062330067692));
#8731=DIRECTION('',(-0.999876649514697,0.,0.0157062330067692));
#8732=DIRECTION('',(0.,1.,0.));
#8733=DIRECTION('center_axis',(-0.957469564385932,0.,0.288534284400681));
#8734=DIRECTION('ref_axis',(0.288534284400681,0.,0.957469564385932));
#8735=DIRECTION('',(-0.288534284400681,0.,-0.957469564385932));
#8736=DIRECTION('',(0.288534284400681,0.,0.957469564385932));
#8737=DIRECTION('',(0.,1.,0.));
#8738=DIRECTION('center_axis',(0.24361606355275,0.,-0.969871751098599));
#8739=DIRECTION('ref_axis',(-0.969871751098599,0.,-0.24361606355275));
#8740=DIRECTION('',(0.969871751098599,0.,0.24361606355275));
#8741=DIRECTION('',(-0.969871751098599,0.,-0.24361606355275));
#8742=DIRECTION('',(0.,1.,0.));
#8743=DIRECTION('center_axis',(-0.999522748094039,0.,0.0308913587033594));
#8744=DIRECTION('ref_axis',(0.0308913587033594,0.,0.999522748094039));
#8745=DIRECTION('',(-0.0308913587033594,0.,-0.999522748094039));
#8746=DIRECTION('',(0.0308913587033594,0.,0.999522748094039));
#8747=DIRECTION('',(0.,1.,0.));
#8748=DIRECTION('center_axis',(0.486336327975727,0.,-0.873771695633983));
#8749=DIRECTION('ref_axis',(-0.873771695633983,0.,-0.486336327975727));
#8750=DIRECTION('',(0.873771695633983,0.,0.486336327975727));
#8751=DIRECTION('',(-0.873771695633983,0.,-0.486336327975727));
#8752=DIRECTION('',(0.,1.,0.));
#8753=DIRECTION('center_axis',(-0.973460108308978,0.,-0.228856762039212));
#8754=DIRECTION('ref_axis',(-0.228856762039212,0.,0.973460108308978));
#8755=DIRECTION('',(0.228856762039212,0.,-0.973460108308978));
#8756=DIRECTION('',(-0.228856762039212,0.,0.973460108308978));
#8757=DIRECTION('',(0.,1.,0.));
#8758=DIRECTION('center_axis',(0.695913575355945,0.,-0.718125543087909));
#8759=DIRECTION('ref_axis',(-0.718125543087909,0.,-0.695913575355945));
#8760=DIRECTION('',(0.718125543087909,0.,0.695913575355945));
#8761=DIRECTION('',(-0.718125543087909,0.,-0.695913575355945));
#8762=DIRECTION('',(0.,1.,0.));
#8763=DIRECTION('center_axis',(-0.881057770861552,0.,-0.473008672652493));
#8764=DIRECTION('ref_axis',(-0.473008672652493,0.,0.881057770861552));
#8765=DIRECTION('',(0.473008672652493,0.,-0.881057770861552));
#8766=DIRECTION('',(-0.473008672652493,0.,0.881057770861552));
#8767=DIRECTION('',(0.,1.,0.));
#8768=DIRECTION('center_axis',(0.858065462627214,0.,-0.513540321538968));
#8769=DIRECTION('ref_axis',(-0.513540321538968,0.,-0.858065462627214));
#8770=DIRECTION('',(0.513540321538968,0.,0.858065462627214));
#8771=DIRECTION('',(-0.513540321538968,0.,-0.858065462627214));
#8772=DIRECTION('',(0.,1.,0.));
#8773=DIRECTION('center_axis',(-0.728612802346719,0.,-0.684925823908298));
#8774=DIRECTION('ref_axis',(-0.684925823908298,0.,0.728612802346719));
#8775=DIRECTION('',(0.684925823908298,0.,-0.728612802346719));
#8776=DIRECTION('',(-0.684925823908298,0.,0.728612802346719));
#8777=DIRECTION('',(0.,1.,0.));
#8778=DIRECTION('center_axis',(0.96174160664066,0.,-0.273958175742653));
#8779=DIRECTION('ref_axis',(-0.273958175742653,0.,-0.96174160664066));
#8780=DIRECTION('',(0.273958175742653,0.,0.96174160664066));
#8781=DIRECTION('',(-0.273958175742653,0.,-0.96174160664066));
#8782=DIRECTION('',(0.,1.,0.));
#8783=DIRECTION('center_axis',(-0.526514075441546,0.,-0.850166412158193));
#8784=DIRECTION('ref_axis',(-0.850166412158193,0.,0.526514075441546));
#8785=DIRECTION('',(0.850166412158193,0.,-0.526514075441546));
#8786=DIRECTION('',(-0.850166412158193,0.,0.526514075441546));
#8787=DIRECTION('',(0.,1.,0.));
#8788=DIRECTION('center_axis',(0.999876649514698,0.,-0.0157062330067686));
#8789=DIRECTION('ref_axis',(-0.0157062330067686,0.,-0.999876649514698));
#8790=DIRECTION('',(0.0157062330067686,0.,0.999876649514698));
#8791=DIRECTION('',(-0.0157062330067686,0.,-0.999876649514698));
#8792=DIRECTION('',(0.,1.,0.));
#8793=DIRECTION('center_axis',(-0.288534284400682,0.,-0.957469564385932));
#8794=DIRECTION('ref_axis',(-0.957469564385932,0.,0.288534284400682));
#8795=DIRECTION('',(0.957469564385932,0.,-0.288534284400682));
#8796=DIRECTION('',(-0.957469564385932,0.,0.288534284400682));
#8797=DIRECTION('',(0.,1.,0.));
#8798=DIRECTION('center_axis',(0.969871751098599,0.,0.24361606355275));
#8799=DIRECTION('ref_axis',(0.24361606355275,0.,-0.969871751098599));
#8800=DIRECTION('',(-0.24361606355275,0.,0.969871751098599));
#8801=DIRECTION('',(0.24361606355275,0.,-0.969871751098599));
#8802=DIRECTION('',(0.,1.,0.));
#8803=DIRECTION('center_axis',(-0.0308913587033594,0.,-0.999522748094039));
#8804=DIRECTION('ref_axis',(-0.999522748094039,0.,0.0308913587033594));
#8805=DIRECTION('',(0.999522748094039,0.,-0.0308913587033594));
#8806=DIRECTION('',(-0.999522748094039,0.,0.0308913587033594));
#8807=DIRECTION('',(0.,1.,0.));
#8808=DIRECTION('center_axis',(0.873771695633986,0.,0.486336327975723));
#8809=DIRECTION('ref_axis',(0.486336327975723,0.,-0.873771695633986));
#8810=DIRECTION('',(-0.486336327975723,0.,0.873771695633986));
#8811=DIRECTION('',(0.486336327975723,0.,-0.873771695633986));
#8812=DIRECTION('',(0.,1.,0.));
#8813=DIRECTION('center_axis',(0.228856762039213,0.,-0.973460108308978));
#8814=DIRECTION('ref_axis',(-0.973460108308978,0.,-0.228856762039213));
#8815=DIRECTION('',(0.973460108308978,0.,0.228856762039213));
#8816=DIRECTION('',(-0.973460108308978,0.,-0.228856762039213));
#8817=DIRECTION('',(0.,1.,0.));
#8818=DIRECTION('center_axis',(0.718125543087909,0.,0.695913575355946));
#8819=DIRECTION('ref_axis',(0.695913575355946,0.,-0.718125543087909));
#8820=DIRECTION('',(-0.695913575355946,0.,0.718125543087909));
#8821=DIRECTION('',(0.695913575355946,0.,-0.718125543087909));
#8822=DIRECTION('',(0.,1.,0.));
#8823=DIRECTION('center_axis',(0.473008672652493,0.,-0.881057770861552));
#8824=DIRECTION('ref_axis',(-0.881057770861552,0.,-0.473008672652493));
#8825=DIRECTION('',(0.881057770861552,0.,0.473008672652493));
#8826=DIRECTION('',(-0.881057770861552,0.,-0.473008672652493));
#8827=DIRECTION('',(0.,1.,0.));
#8828=DIRECTION('center_axis',(0.513540321538969,0.,0.858065462627213));
#8829=DIRECTION('ref_axis',(0.858065462627213,0.,-0.513540321538969));
#8830=DIRECTION('',(-0.858065462627213,0.,0.513540321538969));
#8831=DIRECTION('',(0.858065462627213,0.,-0.513540321538969));
#8832=DIRECTION('',(0.,1.,0.));
#8833=DIRECTION('center_axis',(0.684925823908296,0.,-0.728612802346721));
#8834=DIRECTION('ref_axis',(-0.728612802346721,0.,-0.684925823908296));
#8835=DIRECTION('',(0.728612802346721,0.,0.684925823908296));
#8836=DIRECTION('',(-0.728612802346721,0.,-0.684925823908296));
#8837=DIRECTION('',(0.,1.,0.));
#8838=DIRECTION('center_axis',(0.27395817574266,0.,0.961741606640658));
#8839=DIRECTION('ref_axis',(0.961741606640658,0.,-0.27395817574266));
#8840=DIRECTION('',(-0.961741606640658,0.,0.27395817574266));
#8841=DIRECTION('',(0.961741606640658,0.,-0.27395817574266));
#8842=DIRECTION('',(0.,1.,0.));
#8843=DIRECTION('center_axis',(0.850166412158193,0.,-0.526514075441546));
#8844=DIRECTION('ref_axis',(-0.526514075441546,0.,-0.850166412158193));
#8845=DIRECTION('',(0.526514075441546,0.,0.850166412158193));
#8846=DIRECTION('',(-0.526514075441546,0.,-0.850166412158193));
#8847=DIRECTION('center_axis',(0.,1.,0.));
#8848=DIRECTION('ref_axis',(0.,0.,1.));
#8849=DIRECTION('center_axis',(0.,1.,0.));
#8850=DIRECTION('ref_axis',(1.,0.,0.));
#8851=DIRECTION('axis',(0.,0.,1.));
#8852=DIRECTION('refdir',(1.,0.,0.));
#8853=DIRECTION('center_axis',(0.,1.,0.));
#8854=DIRECTION('ref_axis',(1.,0.,0.));
#8855=DIRECTION('center_axis',(0.,1.,0.));
#8856=DIRECTION('ref_axis',(1.,0.,0.));
#8857=DIRECTION('',(0.,1.,0.));
#8858=DIRECTION('center_axis',(0.,-1.,0.));
#8859=DIRECTION('ref_axis',(1.,0.,0.));
#8860=DIRECTION('center_axis',(0.,0.,1.));
#8861=DIRECTION('ref_axis',(1.,0.,0.));
#8862=DIRECTION('',(0.,1.,0.));
#8863=DIRECTION('center_axis',(0.,0.,1.));
#8864=DIRECTION('ref_axis',(1.,0.,0.));
#8865=DIRECTION('center_axis',(0.,0.,1.));
#8866=DIRECTION('ref_axis',(1.,0.,0.));
#8867=DIRECTION('center_axis',(0.,0.,1.));
#8868=DIRECTION('ref_axis',(1.,0.,0.));
#8869=DIRECTION('',(0.,0.,1.));
#8870=DIRECTION('center_axis',(0.,0.,1.));
#8871=DIRECTION('ref_axis',(1.,0.,0.));
#8872=DIRECTION('center_axis',(0.,0.,1.));
#8873=DIRECTION('ref_axis',(1.,0.,0.));
#8874=DIRECTION('center_axis',(0.,0.,1.));
#8875=DIRECTION('ref_axis',(1.,0.,0.));
#8876=DIRECTION('center_axis',(0.,0.,1.));
#8877=DIRECTION('ref_axis',(1.,0.,0.));
#8878=DIRECTION('',(0.,-1.,0.));
#8879=DIRECTION('center_axis',(0.,1.,0.));
#8880=DIRECTION('ref_axis',(1.,0.,0.));
#8881=DIRECTION('center_axis',(0.,1.,0.));
#8882=DIRECTION('ref_axis',(1.,0.,0.));
#8883=DIRECTION('',(0.,0.,1.));
#8884=DIRECTION('',(-1.,0.,0.));
#8885=DIRECTION('',(0.,0.,-1.));
#8886=DIRECTION('center_axis',(0.,1.,0.));
#8887=DIRECTION('ref_axis',(1.,0.,0.));
#8888=DIRECTION('center_axis',(0.,-1.,0.));
#8889=DIRECTION('ref_axis',(1.,0.,0.));
#8890=DIRECTION('center_axis',(-1.,0.,0.));
#8891=DIRECTION('ref_axis',(0.,0.,1.));
#8892=DIRECTION('',(0.,1.,0.));
#8893=DIRECTION('',(0.,1.,0.));
#8894=DIRECTION('',(0.,0.,1.));
#8895=DIRECTION('center_axis',(0.,1.,0.));
#8896=DIRECTION('ref_axis',(0.,0.,1.));
#8897=DIRECTION('center_axis',(0.,1.,0.));
#8898=DIRECTION('ref_axis',(1.,0.,0.));
#8899=DIRECTION('',(1.,0.,0.));
#8900=DIRECTION('',(0.,0.,-1.));
#8901=DIRECTION('center_axis',(1.,0.,0.));
#8902=DIRECTION('ref_axis',(0.,0.,-1.));
#8903=DIRECTION('',(0.,-1.,0.));
#8904=DIRECTION('',(0.,1.,0.));
#8905=DIRECTION('center_axis',(0.,0.,1.));
#8906=DIRECTION('ref_axis',(1.,0.,0.));
#8907=DIRECTION('center_axis',(0.,1.,0.));
#8908=DIRECTION('ref_axis',(1.,0.,0.));
#8909=DIRECTION('center_axis',(0.,1.,0.));
#8910=DIRECTION('ref_axis',(1.,0.,0.));
#8911=DIRECTION('',(0.,-1.,0.));
#8912=DIRECTION('center_axis',(0.,1.,0.));
#8913=DIRECTION('ref_axis',(1.,0.,0.));
#8914=DIRECTION('center_axis',(0.,-1.,0.));
#8915=DIRECTION('ref_axis',(1.,0.,0.));
#8916=DIRECTION('',(0.,-1.,0.));
#8917=DIRECTION('center_axis',(0.,1.,0.));
#8918=DIRECTION('ref_axis',(1.,0.,0.));
#8919=DIRECTION('axis',(0.,0.,1.));
#8920=DIRECTION('refdir',(1.,0.,0.));
#8921=DIRECTION('center_axis',(0.,1.,0.));
#8922=DIRECTION('ref_axis',(1.,0.,0.));
#8923=DIRECTION('center_axis',(0.,1.,0.));
#8924=DIRECTION('ref_axis',(1.,0.,0.));
#8925=DIRECTION('',(0.,1.,0.));
#8926=DIRECTION('center_axis',(0.,-1.,0.));
#8927=DIRECTION('ref_axis',(1.,0.,0.));
#8928=DIRECTION('center_axis',(0.,1.,0.));
#8929=DIRECTION('ref_axis',(1.,0.,0.));
#8930=DIRECTION('center_axis',(0.,1.,0.));
#8931=DIRECTION('ref_axis',(1.,0.,0.));
#8932=DIRECTION('center_axis',(0.,1.,0.));
#8933=DIRECTION('ref_axis',(1.,0.,0.));
#8934=DIRECTION('',(0.,-1.,0.));
#8935=DIRECTION('center_axis',(0.,1.,0.));
#8936=DIRECTION('ref_axis',(1.,0.,0.));
#8937=DIRECTION('center_axis',(0.,1.,0.));
#8938=DIRECTION('ref_axis',(1.,0.,0.));
#8939=DIRECTION('center_axis',(0.,1.,0.));
#8940=DIRECTION('ref_axis',(1.,0.,0.));
#8941=DIRECTION('axis',(0.,0.,1.));
#8942=DIRECTION('refdir',(1.,0.,0.));
#8943=DIRECTION('center_axis',(0.866025403784439,0.,-0.5));
#8944=DIRECTION('ref_axis',(0.5,0.,0.866025403784439));
#8945=DIRECTION('',(0.5,0.,0.866025403784439));
#8946=DIRECTION('',(0.,-1.,0.));
#8947=DIRECTION('',(0.5,0.,0.866025403784439));
#8948=DIRECTION('',(0.,-1.,0.));
#8949=DIRECTION('center_axis',(1.92296268638356E-16,0.,-1.));
#8950=DIRECTION('ref_axis',(1.,0.,1.92296268638356E-16));
#8951=DIRECTION('',(1.,0.,1.92296268638356E-16));
#8952=DIRECTION('',(0.,-1.,0.));
#8953=DIRECTION('',(1.,0.,1.92296268638356E-16));
#8954=DIRECTION('center_axis',(-0.866025403784439,0.,-0.5));
#8955=DIRECTION('ref_axis',(0.5,0.,-0.866025403784439));
#8956=DIRECTION('',(0.5,0.,-0.866025403784439));
#8957=DIRECTION('',(0.,-1.,0.));
#8958=DIRECTION('',(0.5,0.,-0.866025403784438));
#8959=DIRECTION('center_axis',(-0.866025403784439,0.,0.5));
#8960=DIRECTION('ref_axis',(-0.5,0.,-0.866025403784439));
#8961=DIRECTION('',(-0.5,0.,-0.866025403784439));
#8962=DIRECTION('',(0.,-1.,0.));
#8963=DIRECTION('',(-0.5,0.,-0.866025403784439));
#8964=DIRECTION('center_axis',(-1.92296268638356E-16,0.,1.));
#8965=DIRECTION('ref_axis',(-1.,0.,-1.92296268638356E-16));
#8966=DIRECTION('',(-1.,0.,-1.92296268638356E-16));
#8967=DIRECTION('',(0.,-1.,0.));
#8968=DIRECTION('',(-1.,0.,-1.92296268638356E-16));
#8969=DIRECTION('center_axis',(0.866025403784439,0.,0.5));
#8970=DIRECTION('ref_axis',(-0.5,0.,0.866025403784439));
#8971=DIRECTION('',(-0.5,0.,0.866025403784439));
#8972=DIRECTION('',(-0.5,0.,0.866025403784439));
#8973=DIRECTION('center_axis',(0.,-1.,0.));
#8974=DIRECTION('ref_axis',(0.,0.,-1.));
#8975=DIRECTION('center_axis',(0.,1.,0.));
#8976=DIRECTION('ref_axis',(0.,0.,1.));
#8977=DIRECTION('center_axis',(0.,-1.,0.));
#8978=DIRECTION('ref_axis',(1.,0.,0.));
#8979=DIRECTION('center_axis',(0.,-1.,0.));
#8980=DIRECTION('ref_axis',(1.,0.,0.));
#8981=DIRECTION('center_axis',(0.,-1.,0.));
#8982=DIRECTION('ref_axis',(1.,0.,0.));
#8983=DIRECTION('',(0.707106781186547,0.707106781186548,8.65956056235493E-17));
#8984=DIRECTION('center_axis',(0.,-1.,0.));
#8985=DIRECTION('ref_axis',(1.,0.,0.));
#8986=DIRECTION('center_axis',(0.,1.,0.));
#8987=DIRECTION('ref_axis',(1.,0.,0.));
#8988=DIRECTION('',(0.,1.,0.));
#8989=DIRECTION('center_axis',(0.,1.,0.));
#8990=DIRECTION('ref_axis',(1.,0.,0.));
#8991=DIRECTION('center_axis',(0.,-1.,0.));
#8992=DIRECTION('ref_axis',(1.,0.,0.));
#8993=DIRECTION('',(-0.707106781186547,0.707106781186548,-8.65956056235493E-17));
#8994=DIRECTION('center_axis',(0.,-1.,0.));
#8995=DIRECTION('ref_axis',(0.,0.,-1.));
#8996=DIRECTION('axis',(0.,0.,1.));
#8997=DIRECTION('refdir',(1.,0.,0.));
#8998=DIRECTION('center_axis',(0.,1.,0.));
#8999=DIRECTION('ref_axis',(0.,0.,1.));
#9000=DIRECTION('center_axis',(0.,-1.,0.));
#9001=DIRECTION('ref_axis',(1.,0.,0.));
#9002=DIRECTION('center_axis',(0.,-1.,0.));
#9003=DIRECTION('ref_axis',(1.,0.,0.));
#9004=DIRECTION('center_axis',(0.,-1.,0.));
#9005=DIRECTION('ref_axis',(1.,0.,0.));
#9006=DIRECTION('',(0.707106781186548,0.707106781186547,8.65956056235493E-17));
#9007=DIRECTION('center_axis',(0.,-1.,0.));
#9008=DIRECTION('ref_axis',(1.,0.,0.));
#9009=DIRECTION('center_axis',(0.,-1.,0.));
#9010=DIRECTION('ref_axis',(1.,0.,0.));
#9011=DIRECTION('',(0.,1.,0.));
#9012=DIRECTION('center_axis',(0.,1.,0.));
#9013=DIRECTION('ref_axis',(1.,0.,0.));
#9014=DIRECTION('center_axis',(0.,-1.,0.));
#9015=DIRECTION('ref_axis',(1.,0.,0.));
#9016=DIRECTION('',(-0.707106781186547,0.707106781186548,-8.65956056235493E-17));
#9017=DIRECTION('center_axis',(0.,-1.,0.));
#9018=DIRECTION('ref_axis',(0.,0.,-1.));
#9019=DIRECTION('center_axis',(0.,-1.,0.));
#9020=DIRECTION('ref_axis',(1.,0.,0.));
#9021=DIRECTION('center_axis',(0.,1.,0.));
#9022=DIRECTION('ref_axis',(1.,0.,0.));
#9023=DIRECTION('center_axis',(0.,1.,0.));
#9024=DIRECTION('ref_axis',(1.,0.,0.));
#9025=DIRECTION('',(-0.447213595499958,0.894427190999916,-5.47678698264203E-17));
#9026=DIRECTION('center_axis',(0.,-1.,0.));
#9027=DIRECTION('ref_axis',(1.,0.,0.));
#9028=DIRECTION('center_axis',(0.,1.,0.));
#9029=DIRECTION('ref_axis',(1.,0.,0.));
#9030=DIRECTION('',(0.,1.,0.));
#9031=DIRECTION('center_axis',(0.,1.,0.));
#9032=DIRECTION('ref_axis',(1.,0.,0.));
#9033=DIRECTION('center_axis',(0.,-1.,0.));
#9034=DIRECTION('ref_axis',(1.,0.,0.));
#9035=DIRECTION('',(-0.707106781186547,0.707106781186548,-8.65956056235493E-17));
#9036=DIRECTION('center_axis',(0.,-1.,0.));
#9037=DIRECTION('ref_axis',(0.,0.,-1.));
#9038=DIRECTION('center_axis',(0.866025403784439,0.,-0.5));
#9039=DIRECTION('ref_axis',(0.5,0.,0.866025403784439));
#9040=DIRECTION('',(-0.5,0.,-0.866025403784439));
#9041=DIRECTION('',(0.,-1.,0.));
#9042=DIRECTION('',(0.5,0.,0.866025403784439));
#9043=DIRECTION('',(0.,-1.,0.));
#9044=DIRECTION('center_axis',(1.20185167898973E-16,0.,-1.));
#9045=DIRECTION('ref_axis',(1.,0.,1.20185167898973E-16));
#9046=DIRECTION('',(-1.,0.,-1.20185167898973E-16));
#9047=DIRECTION('',(0.,-1.,0.));
#9048=DIRECTION('',(1.,0.,1.20185167898973E-16));
#9049=DIRECTION('center_axis',(-0.866025403784439,0.,-0.5));
#9050=DIRECTION('ref_axis',(0.5,0.,-0.866025403784439));
#9051=DIRECTION('',(-0.5,0.,0.866025403784439));
#9052=DIRECTION('',(0.,-1.,0.));
#9053=DIRECTION('',(0.5,0.,-0.866025403784439));
#9054=DIRECTION('center_axis',(-0.866025403784439,0.,0.5));
#9055=DIRECTION('ref_axis',(-0.5,0.,-0.866025403784439));
#9056=DIRECTION('',(0.5,0.,0.866025403784439));
#9057=DIRECTION('',(0.,-1.,0.));
#9058=DIRECTION('',(-0.5,0.,-0.866025403784439));
#9059=DIRECTION('center_axis',(-2.40370335797945E-16,0.,1.));
#9060=DIRECTION('ref_axis',(-1.,0.,-2.40370335797945E-16));
#9061=DIRECTION('',(1.,0.,2.40370335797945E-16));
#9062=DIRECTION('',(0.,-1.,0.));
#9063=DIRECTION('',(-1.,0.,-2.40370335797945E-16));
#9064=DIRECTION('center_axis',(0.866025403784439,0.,0.5));
#9065=DIRECTION('ref_axis',(-0.5,0.,0.866025403784439));
#9066=DIRECTION('',(0.5,0.,-0.866025403784439));
#9067=DIRECTION('',(-0.5,0.,0.866025403784439));
#9068=DIRECTION('center_axis',(0.,1.,0.));
#9069=DIRECTION('ref_axis',(1.,0.,0.));
#9070=DIRECTION('center_axis',(0.,-1.,0.));
#9071=DIRECTION('ref_axis',(0.,0.,-1.));
#9072=DIRECTION('',(0.,0.,1.));
#9073=DIRECTION('',(1.,0.,0.));
#9074=DIRECTION('',(0.,0.,1.));
#9075=DIRECTION('',(1.,0.,0.));
#9076=DIRECTION('',(0.,0.,1.));
#9077=DIRECTION('',(1.,0.,0.));
#9078=DIRECTION('',(0.,0.,1.));
#9079=DIRECTION('',(1.,0.,0.));
#9080=DIRECTION('',(0.,0.,1.));
#9081=DIRECTION('',(1.,0.,0.));
#9082=DIRECTION('',(0.,0.,1.));
#9083=DIRECTION('',(1.,0.,0.));
#9084=DIRECTION('',(0.,0.,1.));
#9085=DIRECTION('',(1.,0.,0.));
#9086=DIRECTION('',(0.,0.,1.));
#9087=DIRECTION('',(1.,0.,0.));
#9088=DIRECTION('',(0.,0.,1.));
#9089=DIRECTION('',(1.,0.,0.));
#9090=DIRECTION('',(0.,0.,1.));
#9091=DIRECTION('',(1.,0.,0.));
#9092=DIRECTION('',(0.,0.,1.));
#9093=DIRECTION('',(1.,0.,0.));
#9094=DIRECTION('',(0.,0.,1.));
#9095=DIRECTION('',(1.,0.,0.));
#9096=DIRECTION('',(0.,0.,1.));
#9097=DIRECTION('',(1.,0.,0.));
#9098=DIRECTION('',(0.,0.,1.));
#9099=DIRECTION('',(1.,0.,0.));
#9100=DIRECTION('',(0.,0.,1.));
#9101=DIRECTION('',(1.,0.,0.));
#9102=DIRECTION('',(0.,-1.,2.22044604925031E-16));
#9103=DIRECTION('',(1.,0.,0.));
#9104=DIRECTION('',(0.,-1.,2.22044604925031E-16));
#9105=DIRECTION('',(1.,0.,0.));
#9106=DIRECTION('',(0.,-1.,2.22044604925031E-16));
#9107=DIRECTION('',(1.,0.,0.));
#9108=DIRECTION('',(0.,-1.,2.22044604925031E-16));
#9109=DIRECTION('',(1.,0.,0.));
#9110=DIRECTION('',(0.,0.,1.));
#9111=DIRECTION('',(1.,0.,0.));
#9112=DIRECTION('',(0.,-1.,2.22044604925031E-16));
#9113=DIRECTION('',(1.,0.,0.));
#9114=DIRECTION('',(0.,-1.,2.22044604925031E-16));
#9115=DIRECTION('',(1.,0.,0.));
#9116=DIRECTION('',(0.,-1.,2.22044604925031E-16));
#9117=DIRECTION('',(1.,0.,0.));
#9118=DIRECTION('',(0.,-1.,2.22044604925031E-16));
#9119=DIRECTION('',(1.,0.,0.));
#9120=DIRECTION('',(0.,-1.,2.22044604925031E-16));
#9121=DIRECTION('',(1.,0.,0.));
#9122=DIRECTION('',(0.,-1.,2.22044604925031E-16));
#9123=DIRECTION('',(1.,0.,0.));
#9124=DIRECTION('',(0.,-1.,2.22044604925031E-16));
#9125=DIRECTION('',(1.,0.,0.));
#9126=DIRECTION('',(0.,-1.,2.22044604925031E-16));
#9127=DIRECTION('',(1.,0.,0.));
#9128=DIRECTION('',(0.,0.,1.));
#9129=DIRECTION('',(1.,0.,0.));
#9130=DIRECTION('',(0.,-1.,2.22044604925031E-16));
#9131=DIRECTION('',(1.,0.,0.));
#9132=DIRECTION('',(0.,-1.,2.22044604925031E-16));
#9133=DIRECTION('',(1.,0.,0.));
#9134=DIRECTION('',(0.,-1.,2.22044604925031E-16));
#9135=DIRECTION('',(1.,0.,0.));
#9136=DIRECTION('',(0.,-1.,2.22044604925031E-16));
#9137=DIRECTION('',(1.,0.,0.));
#9138=DIRECTION('',(0.,-1.,2.22044604925031E-16));
#9139=DIRECTION('',(1.,0.,0.));
#9140=DIRECTION('',(0.,-1.,2.22044604925031E-16));
#9141=DIRECTION('',(1.,0.,0.));
#9142=DIRECTION('',(0.,0.,1.));
#9143=DIRECTION('',(1.,0.,0.));
#9144=DIRECTION('',(0.,-1.,2.22044604925031E-16));
#9145=DIRECTION('',(1.,0.,0.));
#9146=DIRECTION('',(0.,0.,1.));
#9147=DIRECTION('',(1.,0.,0.));
#9148=DIRECTION('',(0.,0.,1.));
#9149=DIRECTION('',(1.,0.,0.));
#9150=DIRECTION('',(0.,0.,1.));
#9151=DIRECTION('',(1.,0.,0.));
#9152=DIRECTION('',(0.,0.,1.));
#9153=DIRECTION('',(1.,0.,0.));
#9154=DIRECTION('',(0.,0.,1.));
#9155=DIRECTION('',(1.,0.,0.));
#9156=DIRECTION('',(0.,0.,1.));
#9157=DIRECTION('',(1.,0.,0.));
#9158=DIRECTION('',(0.,0.,1.));
#9159=DIRECTION('',(1.,0.,0.));
#9160=DIRECTION('',(0.,0.,1.));
#9161=DIRECTION('',(1.,0.,0.));
#9162=DIRECTION('',(0.,0.,1.));
#9163=DIRECTION('',(1.,0.,0.));
#9164=DIRECTION('',(0.,0.,1.));
#9165=DIRECTION('',(1.,0.,0.));
#9166=DIRECTION('',(0.,0.,1.));
#9167=DIRECTION('',(1.,0.,0.));
#9168=DIRECTION('',(0.,-1.,2.22044604925031E-16));
#9169=DIRECTION('',(1.,0.,0.));
#9170=DIRECTION('',(0.,-1.,2.22044604925031E-16));
#9171=DIRECTION('',(1.,0.,0.));
#9172=DIRECTION('',(0.,-1.,2.22044604925031E-16));
#9173=DIRECTION('',(1.,0.,0.));
#9174=DIRECTION('',(0.,-1.,2.22044604925031E-16));
#9175=DIRECTION('',(1.,0.,0.));
#9176=DIRECTION('',(0.,-1.,2.22044604925031E-16));
#9177=DIRECTION('',(1.,0.,0.));
#9178=DIRECTION('',(0.,-1.,2.22044604925031E-16));
#9179=DIRECTION('',(1.,0.,0.));
#9180=DIRECTION('',(0.,0.,1.));
#9181=DIRECTION('',(1.,0.,0.));
#9182=DIRECTION('axis',(0.,0.,1.));
#9183=DIRECTION('refdir',(1.,0.,0.));
#9184=DIRECTION('axis',(0.,0.,1.));
#9185=DIRECTION('refdir',(1.,0.,0.));
#9186=DIRECTION('center_axis',(0.,1.,0.));
#9187=DIRECTION('ref_axis',(1.,0.,0.));
#9188=DIRECTION('center_axis',(0.,1.,0.));
#9189=DIRECTION('ref_axis',(1.,0.,0.));
#9190=DIRECTION('',(0.,1.,0.));
#9191=DIRECTION('center_axis',(0.,-1.,0.));
#9192=DIRECTION('ref_axis',(1.,0.,0.));
#9193=DIRECTION('center_axis',(0.,1.,0.));
#9194=DIRECTION('ref_axis',(0.185131832090925,0.,0.982713694189034));
#9195=DIRECTION('',(0.,1.,0.));
#9196=DIRECTION('center_axis',(0.,1.,0.));
#9197=DIRECTION('ref_axis',(1.,0.,0.));
#9198=DIRECTION('',(0.,-1.,0.));
#9199=DIRECTION('center_axis',(0.,1.,0.));
#9200=DIRECTION('ref_axis',(1.,0.,0.));
#9201=DIRECTION('center_axis',(-0.862655693448417,0.,0.50579161179386));
#9202=DIRECTION('ref_axis',(0.50579161179386,0.,0.862655693448417));
#9203=DIRECTION('',(0.50579161179386,0.,0.862655693448417));
#9204=DIRECTION('',(0.,1.,0.));
#9205=DIRECTION('',(-0.50579161179386,0.,-0.862655693448417));
#9206=DIRECTION('center_axis',(0.,1.,0.));
#9207=DIRECTION('ref_axis',(0.,0.,1.));
#9208=DIRECTION('',(-0.615893007805892,0.,-0.78782980581837));
#9209=DIRECTION('',(-1.,0.,0.));
#9210=DIRECTION('center_axis',(0.,0.,-1.));
#9211=DIRECTION('ref_axis',(-1.,0.,0.));
#9212=DIRECTION('',(1.,0.,0.));
#9213=DIRECTION('',(0.,1.,0.));
#9214=DIRECTION('center_axis',(0.78782980581837,0.,-0.615893007805892));
#9215=DIRECTION('ref_axis',(-0.615893007805892,0.,-0.78782980581837));
#9216=DIRECTION('',(0.615893007805892,0.,0.78782980581837));
#9217=DIRECTION('center_axis',(0.,1.,0.));
#9218=DIRECTION('ref_axis',(1.,0.,0.));
#9219=DIRECTION('',(0.,0.,1.));
#9220=DIRECTION('',(1.,0.,0.));
#9221=DIRECTION('',(0.,0.,1.));
#9222=DIRECTION('',(1.,0.,0.));
#9223=DIRECTION('',(0.,0.,1.));
#9224=DIRECTION('',(1.,0.,0.));
#9225=DIRECTION('',(0.,0.,1.));
#9226=DIRECTION('',(1.,0.,0.));
#9227=CARTESIAN_POINT('',(0.,0.,0.));
#9228=CARTESIAN_POINT('',(0.,0.,0.));
#9229=CARTESIAN_POINT('',(0.,0.,0.));
#9230=CARTESIAN_POINT('Origin',(8.,-5.9,-0.1));
#9231=CARTESIAN_POINT('',(7.79,-5.9,0.));
#9232=CARTESIAN_POINT('Origin',(8.,-5.9,0.));
#9233=CARTESIAN_POINT('',(7.79,-5.9,1.2));
#9234=CARTESIAN_POINT('',(7.79,-5.9,-0.1));
#9235=CARTESIAN_POINT('Origin',(8.,-5.9,1.2));
#9236=CARTESIAN_POINT('Origin',(5.6,-5.9,-0.1));
#9237=CARTESIAN_POINT('',(5.39,-5.9,0.));
#9238=CARTESIAN_POINT('Origin',(5.6,-5.9,0.));
#9239=CARTESIAN_POINT('',(5.39,-5.9,1.2));
#9240=CARTESIAN_POINT('',(5.39,-5.9,-0.1));
#9241=CARTESIAN_POINT('Origin',(5.6,-5.9,1.2));
#9242=CARTESIAN_POINT('Origin',(5.7,14.5,-0.1));
#9243=CARTESIAN_POINT('',(5.49,14.5,0.));
#9244=CARTESIAN_POINT('Origin',(5.7,14.5,0.));
#9245=CARTESIAN_POINT('',(5.49,14.5,1.2));
#9246=CARTESIAN_POINT('',(5.49,14.5,-0.1));
#9247=CARTESIAN_POINT('Origin',(5.7,14.5,1.2));
#9248=CARTESIAN_POINT('Origin',(5.7,17.5,-0.1));
#9249=CARTESIAN_POINT('',(5.49,17.5,0.));
#9250=CARTESIAN_POINT('Origin',(5.7,17.5,0.));
#9251=CARTESIAN_POINT('',(5.49,17.5,1.2));
#9252=CARTESIAN_POINT('',(5.49,17.5,-0.1));
#9253=CARTESIAN_POINT('Origin',(5.7,17.5,1.2));
#9254=CARTESIAN_POINT('Origin',(-5.7,14.5,-0.1));
#9255=CARTESIAN_POINT('',(-5.91,14.5,0.));
#9256=CARTESIAN_POINT('Origin',(-5.7,14.5,0.));
#9257=CARTESIAN_POINT('',(-5.91,14.5,1.2));
#9258=CARTESIAN_POINT('',(-5.91,14.5,-0.1));
#9259=CARTESIAN_POINT('Origin',(-5.7,14.5,1.2));
#9260=CARTESIAN_POINT('Origin',(-5.7,17.5,-0.1));
#9261=CARTESIAN_POINT('',(-5.91,17.5,0.));
#9262=CARTESIAN_POINT('Origin',(-5.7,17.5,0.));
#9263=CARTESIAN_POINT('',(-5.91,17.5,1.2));
#9264=CARTESIAN_POINT('',(-5.91,17.5,-0.1));
#9265=CARTESIAN_POINT('Origin',(-5.7,17.5,1.2));
#9266=CARTESIAN_POINT('Origin',(5.7,-1.5,-0.1));
#9267=CARTESIAN_POINT('',(5.49,-1.5,0.));
#9268=CARTESIAN_POINT('Origin',(5.7,-1.5,0.));
#9269=CARTESIAN_POINT('',(5.49,-1.5,1.2));
#9270=CARTESIAN_POINT('',(5.49,-1.5,-0.1));
#9271=CARTESIAN_POINT('Origin',(5.7,-1.5,1.2));
#9272=CARTESIAN_POINT('Origin',(5.7,1.5,-0.1));
#9273=CARTESIAN_POINT('',(5.49,1.5,0.));
#9274=CARTESIAN_POINT('Origin',(5.7,1.5,0.));
#9275=CARTESIAN_POINT('',(5.49,1.5,1.2));
#9276=CARTESIAN_POINT('',(5.49,1.5,-0.1));
#9277=CARTESIAN_POINT('Origin',(5.7,1.5,1.2));
#9278=CARTESIAN_POINT('Origin',(-5.7,-1.5,-0.1));
#9279=CARTESIAN_POINT('',(-5.91,-1.5,0.));
#9280=CARTESIAN_POINT('Origin',(-5.7,-1.5,0.));
#9281=CARTESIAN_POINT('',(-5.91,-1.5,1.2));
#9282=CARTESIAN_POINT('',(-5.91,-1.5,-0.1));
#9283=CARTESIAN_POINT('Origin',(-5.7,-1.5,1.2));
#9284=CARTESIAN_POINT('Origin',(-5.7,1.5,-0.1));
#9285=CARTESIAN_POINT('',(-5.91,1.5,0.));
#9286=CARTESIAN_POINT('Origin',(-5.7,1.5,0.));
#9287=CARTESIAN_POINT('',(-5.91,1.5,1.2));
#9288=CARTESIAN_POINT('',(-5.91,1.5,-0.1));
#9289=CARTESIAN_POINT('Origin',(-5.7,1.5,1.2));
#9290=CARTESIAN_POINT('Origin',(10.,20.5,0.));
#9291=CARTESIAN_POINT('',(10.,20.5,0.));
#9292=CARTESIAN_POINT('',(-8.,20.5,0.));
#9293=CARTESIAN_POINT('',(10.,20.5,0.));
#9294=CARTESIAN_POINT('',(-8.,20.5,1.2));
#9295=CARTESIAN_POINT('',(-8.,20.5,0.));
#9296=CARTESIAN_POINT('',(10.,20.5,1.2));
#9297=CARTESIAN_POINT('',(10.,20.5,1.2));
#9298=CARTESIAN_POINT('',(10.,20.5,0.));
#9299=CARTESIAN_POINT('Origin',(10.,-8.5,0.));
#9300=CARTESIAN_POINT('',(10.,-8.5,0.));
#9301=CARTESIAN_POINT('',(10.,-8.5,0.));
#9302=CARTESIAN_POINT('',(10.,-8.5,1.2));
#9303=CARTESIAN_POINT('',(10.,-8.5,1.2));
#9304=CARTESIAN_POINT('',(10.,-8.5,0.));
#9305=CARTESIAN_POINT('Origin',(-8.,-8.5,0.));
#9306=CARTESIAN_POINT('',(-8.,-8.5,0.));
#9307=CARTESIAN_POINT('',(-8.,-8.5,0.));
#9308=CARTESIAN_POINT('',(-8.,-8.5,1.2));
#9309=CARTESIAN_POINT('',(-8.,-8.5,1.2));
#9310=CARTESIAN_POINT('',(-8.,-8.5,0.));
#9311=CARTESIAN_POINT('Origin',(-8.,20.5,0.));
#9312=CARTESIAN_POINT('',(-8.,20.5,0.));
#9313=CARTESIAN_POINT('',(-8.,20.5,1.2));
#9314=CARTESIAN_POINT('Origin',(1.,6.,1.2));
#9315=CARTESIAN_POINT('Origin',(1.,6.,0.));
#9316=CARTESIAN_POINT('',(0.,0.,0.));
#9317=CARTESIAN_POINT('Origin',(10.,-7.5,-0.8));
#9318=CARTESIAN_POINT('',(10.,-7.5,-0.8));
#9319=CARTESIAN_POINT('',(-8.,-7.5,-0.8));
#9320=CARTESIAN_POINT('',(10.,-7.5,-0.8));
#9321=CARTESIAN_POINT('',(-8.,-7.5,0.));
#9322=CARTESIAN_POINT('',(-8.,-7.5,-0.8));
#9323=CARTESIAN_POINT('',(10.,-7.5,0.));
#9324=CARTESIAN_POINT('',(10.,-7.5,0.));
#9325=CARTESIAN_POINT('',(10.,-7.5,-0.8));
#9326=CARTESIAN_POINT('Origin',(10.,-8.5,-0.8));
#9327=CARTESIAN_POINT('',(10.,-8.5,-0.8));
#9328=CARTESIAN_POINT('',(10.,-8.5,-0.8));
#9329=CARTESIAN_POINT('',(10.,-8.5,0.));
#9330=CARTESIAN_POINT('',(10.,-8.5,0.));
#9331=CARTESIAN_POINT('',(10.,-8.5,-0.8));
#9332=CARTESIAN_POINT('Origin',(-8.,-8.5,-0.8));
#9333=CARTESIAN_POINT('',(-8.,-8.5,-0.8));
#9334=CARTESIAN_POINT('',(-8.,-8.5,-0.8));
#9335=CARTESIAN_POINT('',(-8.,-8.5,0.));
#9336=CARTESIAN_POINT('',(-8.,-8.5,0.));
#9337=CARTESIAN_POINT('',(-8.,-8.5,-0.8));
#9338=CARTESIAN_POINT('Origin',(-8.,-7.5,-0.8));
#9339=CARTESIAN_POINT('',(-8.,-7.5,-0.8));
#9340=CARTESIAN_POINT('',(-8.,-7.5,0.));
#9341=CARTESIAN_POINT('Origin',(1.,-8.,0.));
#9342=CARTESIAN_POINT('Origin',(1.,-8.,-0.8));
#9343=CARTESIAN_POINT('',(0.,0.,0.));
#9344=CARTESIAN_POINT('Origin',(10.,20.5,-0.8));
#9345=CARTESIAN_POINT('',(10.,20.5,-0.8));
#9346=CARTESIAN_POINT('',(-8.,20.5,-0.8));
#9347=CARTESIAN_POINT('',(10.,20.5,-0.8));
#9348=CARTESIAN_POINT('',(-8.,20.5,0.));
#9349=CARTESIAN_POINT('',(-8.,20.5,-0.8));
#9350=CARTESIAN_POINT('',(10.,20.5,0.));
#9351=CARTESIAN_POINT('',(10.,20.5,0.));
#9352=CARTESIAN_POINT('',(10.,20.5,-0.8));
#9353=CARTESIAN_POINT('Origin',(10.,19.5,-0.8));
#9354=CARTESIAN_POINT('',(10.,19.5,-0.8));
#9355=CARTESIAN_POINT('',(10.,19.5,-0.8));
#9356=CARTESIAN_POINT('',(10.,19.5,0.));
#9357=CARTESIAN_POINT('',(10.,19.5,0.));
#9358=CARTESIAN_POINT('',(10.,19.5,-0.8));
#9359=CARTESIAN_POINT('Origin',(-8.,19.5,-0.8));
#9360=CARTESIAN_POINT('',(-8.,19.5,-0.8));
#9361=CARTESIAN_POINT('',(-8.,19.5,-0.8));
#9362=CARTESIAN_POINT('',(-8.,19.5,0.));
#9363=CARTESIAN_POINT('',(-8.,19.5,0.));
#9364=CARTESIAN_POINT('',(-8.,19.5,-0.8));
#9365=CARTESIAN_POINT('Origin',(-8.,20.5,-0.8));
#9366=CARTESIAN_POINT('',(-8.,20.5,-0.8));
#9367=CARTESIAN_POINT('',(-8.,20.5,0.));
#9368=CARTESIAN_POINT('Origin',(1.,20.,0.));
#9369=CARTESIAN_POINT('Origin',(1.,20.,-0.8));
#9370=CARTESIAN_POINT('',(0.,0.,0.));
#9371=CARTESIAN_POINT('Origin',(5.7,-1.5,2.2));
#9372=CARTESIAN_POINT('',(5.225,-1.5,2.2));
#9373=CARTESIAN_POINT('Origin',(5.7,-1.5,2.2));
#9374=CARTESIAN_POINT('',(5.225,-1.5,3.2));
#9375=CARTESIAN_POINT('',(5.225,-1.5,2.2));
#9376=CARTESIAN_POINT('Origin',(5.7,-1.5,3.2));
#9377=CARTESIAN_POINT('Origin',(5.7,-1.5,2.2));
#9378=CARTESIAN_POINT('',(5.425,-1.5,2.2));
#9379=CARTESIAN_POINT('Origin',(5.7,-1.5,2.2));
#9380=CARTESIAN_POINT('Origin',(5.7,1.5,2.2));
#9381=CARTESIAN_POINT('',(5.225,1.5,2.2));
#9382=CARTESIAN_POINT('Origin',(5.7,1.5,2.2));
#9383=CARTESIAN_POINT('',(5.225,1.5,3.2));
#9384=CARTESIAN_POINT('',(5.225,1.5,2.2));
#9385=CARTESIAN_POINT('Origin',(5.7,1.5,3.2));
#9386=CARTESIAN_POINT('Origin',(5.7,1.5,2.2));
#9387=CARTESIAN_POINT('',(5.425,1.5,2.2));
#9388=CARTESIAN_POINT('Origin',(5.7,1.5,2.2));
#9389=CARTESIAN_POINT('Origin',(5.7,-1.5,1.1));
#9390=CARTESIAN_POINT('',(5.425,-1.5,1.2));
#9391=CARTESIAN_POINT('Origin',(5.7,-1.5,1.2));
#9392=CARTESIAN_POINT('',(5.425,-1.5,1.1));
#9393=CARTESIAN_POINT('Origin',(5.7,1.5,1.1));
#9394=CARTESIAN_POINT('',(5.425,1.5,1.2));
#9395=CARTESIAN_POINT('Origin',(5.7,1.5,1.2));
#9396=CARTESIAN_POINT('',(5.425,1.5,1.1));
#9397=CARTESIAN_POINT('Origin',(-5.7,-1.5,2.2));
#9398=CARTESIAN_POINT('',(-6.175,-1.5,2.2));
#9399=CARTESIAN_POINT('Origin',(-5.7,-1.5,2.2));
#9400=CARTESIAN_POINT('',(-6.175,-1.5,3.2));
#9401=CARTESIAN_POINT('',(-6.175,-1.5,2.2));
#9402=CARTESIAN_POINT('Origin',(-5.7,-1.5,3.2));
#9403=CARTESIAN_POINT('Origin',(-5.7,-1.5,2.2));
#9404=CARTESIAN_POINT('',(-5.975,-1.5,2.2));
#9405=CARTESIAN_POINT('Origin',(-5.7,-1.5,2.2));
#9406=CARTESIAN_POINT('Origin',(-5.7,1.5,2.2));
#9407=CARTESIAN_POINT('',(-6.175,1.5,2.2));
#9408=CARTESIAN_POINT('Origin',(-5.7,1.5,2.2));
#9409=CARTESIAN_POINT('',(-6.175,1.5,3.2));
#9410=CARTESIAN_POINT('',(-6.175,1.5,2.2));
#9411=CARTESIAN_POINT('Origin',(-5.7,1.5,3.2));
#9412=CARTESIAN_POINT('Origin',(-5.7,1.5,2.2));
#9413=CARTESIAN_POINT('',(-5.975,1.5,2.2));
#9414=CARTESIAN_POINT('Origin',(-5.7,1.5,2.2));
#9415=CARTESIAN_POINT('Origin',(-5.7,-1.5,1.1));
#9416=CARTESIAN_POINT('',(-5.975,-1.5,1.2));
#9417=CARTESIAN_POINT('Origin',(-5.7,-1.5,1.2));
#9418=CARTESIAN_POINT('',(-5.975,-1.5,1.1));
#9419=CARTESIAN_POINT('Origin',(-5.7,1.5,1.1));
#9420=CARTESIAN_POINT('',(-5.975,1.5,1.2));
#9421=CARTESIAN_POINT('Origin',(-5.7,1.5,1.2));
#9422=CARTESIAN_POINT('',(-5.975,1.5,1.1));
#9423=CARTESIAN_POINT('Origin',(-4.75,0.,1.1));
#9424=CARTESIAN_POINT('',(-5.09,-4.163799117101E-17,1.2));
#9425=CARTESIAN_POINT('Origin',(-4.75,0.,1.2));
#9426=CARTESIAN_POINT('',(-5.09,4.163799117101E-17,3.2));
#9427=CARTESIAN_POINT('',(-5.09,-4.163799117101E-17,1.1));
#9428=CARTESIAN_POINT('Origin',(-4.75,0.,3.2));
#9429=CARTESIAN_POINT('Origin',(4.75,0.,1.1));
#9430=CARTESIAN_POINT('',(4.41,-4.163799117101E-17,1.2));
#9431=CARTESIAN_POINT('Origin',(4.75,0.,1.2));
#9432=CARTESIAN_POINT('',(4.41,4.163799117101E-17,3.2));
#9433=CARTESIAN_POINT('',(4.41,-4.163799117101E-17,1.1));
#9434=CARTESIAN_POINT('Origin',(4.75,0.,3.2));
#9435=CARTESIAN_POINT('Origin',(6.5,2.2,1.2));
#9436=CARTESIAN_POINT('',(6.5,2.2,1.2));
#9437=CARTESIAN_POINT('',(-6.5,2.2,1.2));
#9438=CARTESIAN_POINT('',(6.5,2.2,1.2));
#9439=CARTESIAN_POINT('',(-6.5,2.2,3.2));
#9440=CARTESIAN_POINT('',(-6.5,2.2,1.2));
#9441=CARTESIAN_POINT('',(6.5,2.2,3.2));
#9442=CARTESIAN_POINT('',(6.5,2.2,3.2));
#9443=CARTESIAN_POINT('',(6.5,2.2,1.2));
#9444=CARTESIAN_POINT('Origin',(6.5,-2.2,1.2));
#9445=CARTESIAN_POINT('',(6.5,-2.2,1.2));
#9446=CARTESIAN_POINT('',(6.5,-2.2,1.2));
#9447=CARTESIAN_POINT('',(6.5,-2.2,3.2));
#9448=CARTESIAN_POINT('',(6.5,-2.2,3.2));
#9449=CARTESIAN_POINT('',(6.5,-2.2,1.2));
#9450=CARTESIAN_POINT('Origin',(-6.5,-2.2,1.2));
#9451=CARTESIAN_POINT('',(-6.5,-2.2,1.2));
#9452=CARTESIAN_POINT('',(-6.5,-2.2,1.2));
#9453=CARTESIAN_POINT('',(-6.5,-2.2,3.2));
#9454=CARTESIAN_POINT('',(-6.5,-2.2,3.2));
#9455=CARTESIAN_POINT('',(-6.5,-2.2,1.2));
#9456=CARTESIAN_POINT('Origin',(-6.5,2.2,1.2));
#9457=CARTESIAN_POINT('',(-6.5,2.2,1.2));
#9458=CARTESIAN_POINT('',(-6.5,2.2,3.2));
#9459=CARTESIAN_POINT('Origin',(0.,0.,3.2));
#9460=CARTESIAN_POINT('Origin',(0.,0.,1.2));
#9461=CARTESIAN_POINT('',(0.,0.,0.));
#9462=CARTESIAN_POINT('Origin',(-4.75,0.,3.2));
#9463=CARTESIAN_POINT('',(-5.175,-5.20474889637625E-17,4.4));
#9464=CARTESIAN_POINT('Origin',(-4.75,0.,4.4));
#9465=CARTESIAN_POINT('',(-5.175,-5.20474889637625E-17,3.2));
#9466=CARTESIAN_POINT('',(-5.175,-5.20474889637625E-17,3.2));
#9467=CARTESIAN_POINT('Origin',(-4.75,0.,3.2));
#9468=CARTESIAN_POINT('Origin',(-4.75,0.,3.2));
#9469=CARTESIAN_POINT('',(-5.395,-7.89897185450042E-17,4.4));
#9470=CARTESIAN_POINT('Origin',(-4.75,0.,4.4));
#9471=CARTESIAN_POINT('',(-5.395,-7.89897185450042E-17,3.2));
#9472=CARTESIAN_POINT('',(-5.395,-7.89897185450042E-17,3.2));
#9473=CARTESIAN_POINT('Origin',(-4.75,0.,3.2));
#9474=CARTESIAN_POINT('Origin',(-4.75,0.,4.4));
#9475=CARTESIAN_POINT('Origin',(-4.75,0.,3.2));
#9476=CARTESIAN_POINT('',(0.,0.,0.));
#9477=CARTESIAN_POINT('Origin',(4.75,0.,3.2));
#9478=CARTESIAN_POINT('',(4.325,-5.20474889637625E-17,4.4));
#9479=CARTESIAN_POINT('Origin',(4.75,0.,4.4));
#9480=CARTESIAN_POINT('',(4.325,-5.20474889637625E-17,3.2));
#9481=CARTESIAN_POINT('',(4.325,-5.20474889637625E-17,3.2));
#9482=CARTESIAN_POINT('Origin',(4.75,0.,3.2));
#9483=CARTESIAN_POINT('Origin',(4.75,0.,3.2));
#9484=CARTESIAN_POINT('',(4.105,-7.89897185450042E-17,4.4));
#9485=CARTESIAN_POINT('Origin',(4.75,0.,4.4));
#9486=CARTESIAN_POINT('',(4.105,-7.89897185450042E-17,3.2));
#9487=CARTESIAN_POINT('',(4.105,-7.89897185450042E-17,3.2));
#9488=CARTESIAN_POINT('Origin',(4.75,0.,3.2));
#9489=CARTESIAN_POINT('Origin',(4.75,0.,4.4));
#9490=CARTESIAN_POINT('Origin',(4.75,0.,3.2));
#9491=CARTESIAN_POINT('',(0.,0.,0.));
#9492=CARTESIAN_POINT('Origin',(5.7,14.5,2.2));
#9493=CARTESIAN_POINT('',(5.225,14.5,2.2));
#9494=CARTESIAN_POINT('Origin',(5.7,14.5,2.2));
#9495=CARTESIAN_POINT('',(5.225,14.5,3.2));
#9496=CARTESIAN_POINT('',(5.225,14.5,2.2));
#9497=CARTESIAN_POINT('Origin',(5.7,14.5,3.2));
#9498=CARTESIAN_POINT('Origin',(5.7,14.5,2.2));
#9499=CARTESIAN_POINT('',(5.425,14.5,2.2));
#9500=CARTESIAN_POINT('Origin',(5.7,14.5,2.2));
#9501=CARTESIAN_POINT('Origin',(5.7,17.5,2.2));
#9502=CARTESIAN_POINT('',(5.225,17.5,2.2));
#9503=CARTESIAN_POINT('Origin',(5.7,17.5,2.2));
#9504=CARTESIAN_POINT('',(5.225,17.5,3.2));
#9505=CARTESIAN_POINT('',(5.225,17.5,2.2));
#9506=CARTESIAN_POINT('Origin',(5.7,17.5,3.2));
#9507=CARTESIAN_POINT('Origin',(5.7,17.5,2.2));
#9508=CARTESIAN_POINT('',(5.425,17.5,2.2));
#9509=CARTESIAN_POINT('Origin',(5.7,17.5,2.2));
#9510=CARTESIAN_POINT('Origin',(5.7,14.5,1.1));
#9511=CARTESIAN_POINT('',(5.425,14.5,1.2));
#9512=CARTESIAN_POINT('Origin',(5.7,14.5,1.2));
#9513=CARTESIAN_POINT('',(5.425,14.5,1.1));
#9514=CARTESIAN_POINT('Origin',(5.7,17.5,1.1));
#9515=CARTESIAN_POINT('',(5.425,17.5,1.2));
#9516=CARTESIAN_POINT('Origin',(5.7,17.5,1.2));
#9517=CARTESIAN_POINT('',(5.425,17.5,1.1));
#9518=CARTESIAN_POINT('Origin',(-5.7,14.5,2.2));
#9519=CARTESIAN_POINT('',(-6.175,14.5,2.2));
#9520=CARTESIAN_POINT('Origin',(-5.7,14.5,2.2));
#9521=CARTESIAN_POINT('',(-6.175,14.5,3.2));
#9522=CARTESIAN_POINT('',(-6.175,14.5,2.2));
#9523=CARTESIAN_POINT('Origin',(-5.7,14.5,3.2));
#9524=CARTESIAN_POINT('Origin',(-5.7,14.5,2.2));
#9525=CARTESIAN_POINT('',(-5.975,14.5,2.2));
#9526=CARTESIAN_POINT('Origin',(-5.7,14.5,2.2));
#9527=CARTESIAN_POINT('Origin',(-5.7,17.5,2.2));
#9528=CARTESIAN_POINT('',(-6.175,17.5,2.2));
#9529=CARTESIAN_POINT('Origin',(-5.7,17.5,2.2));
#9530=CARTESIAN_POINT('',(-6.175,17.5,3.2));
#9531=CARTESIAN_POINT('',(-6.175,17.5,2.2));
#9532=CARTESIAN_POINT('Origin',(-5.7,17.5,3.2));
#9533=CARTESIAN_POINT('Origin',(-5.7,17.5,2.2));
#9534=CARTESIAN_POINT('',(-5.975,17.5,2.2));
#9535=CARTESIAN_POINT('Origin',(-5.7,17.5,2.2));
#9536=CARTESIAN_POINT('Origin',(-5.7,14.5,1.1));
#9537=CARTESIAN_POINT('',(-5.975,14.5,1.2));
#9538=CARTESIAN_POINT('Origin',(-5.7,14.5,1.2));
#9539=CARTESIAN_POINT('',(-5.975,14.5,1.1));
#9540=CARTESIAN_POINT('Origin',(-5.7,17.5,1.1));
#9541=CARTESIAN_POINT('',(-5.975,17.5,1.2));
#9542=CARTESIAN_POINT('Origin',(-5.7,17.5,1.2));
#9543=CARTESIAN_POINT('',(-5.975,17.5,1.1));
#9544=CARTESIAN_POINT('Origin',(-4.75,16.,1.1));
#9545=CARTESIAN_POINT('',(-5.09,16.,1.2));
#9546=CARTESIAN_POINT('Origin',(-4.75,16.,1.2));
#9547=CARTESIAN_POINT('',(-5.09,16.,3.2));
#9548=CARTESIAN_POINT('',(-5.09,16.,1.1));
#9549=CARTESIAN_POINT('Origin',(-4.75,16.,3.2));
#9550=CARTESIAN_POINT('Origin',(4.75,16.,1.1));
#9551=CARTESIAN_POINT('',(4.41,16.,1.2));
#9552=CARTESIAN_POINT('Origin',(4.75,16.,1.2));
#9553=CARTESIAN_POINT('',(4.41,16.,3.2));
#9554=CARTESIAN_POINT('',(4.41,16.,1.1));
#9555=CARTESIAN_POINT('Origin',(4.75,16.,3.2));
#9556=CARTESIAN_POINT('Origin',(6.5,18.2,1.2));
#9557=CARTESIAN_POINT('',(6.5,18.2,1.2));
#9558=CARTESIAN_POINT('',(-6.5,18.2,1.2));
#9559=CARTESIAN_POINT('',(6.5,18.2,1.2));
#9560=CARTESIAN_POINT('',(-6.5,18.2,3.2));
#9561=CARTESIAN_POINT('',(-6.5,18.2,1.2));
#9562=CARTESIAN_POINT('',(6.5,18.2,3.2));
#9563=CARTESIAN_POINT('',(6.5,18.2,3.2));
#9564=CARTESIAN_POINT('',(6.5,18.2,1.2));
#9565=CARTESIAN_POINT('Origin',(6.5,13.8,1.2));
#9566=CARTESIAN_POINT('',(6.5,13.8,1.2));
#9567=CARTESIAN_POINT('',(6.5,13.8,1.2));
#9568=CARTESIAN_POINT('',(6.5,13.8,3.2));
#9569=CARTESIAN_POINT('',(6.5,13.8,3.2));
#9570=CARTESIAN_POINT('',(6.5,13.8,1.2));
#9571=CARTESIAN_POINT('Origin',(-6.5,13.8,1.2));
#9572=CARTESIAN_POINT('',(-6.5,13.8,1.2));
#9573=CARTESIAN_POINT('',(-6.5,13.8,1.2));
#9574=CARTESIAN_POINT('',(-6.5,13.8,3.2));
#9575=CARTESIAN_POINT('',(-6.5,13.8,3.2));
#9576=CARTESIAN_POINT('',(-6.5,13.8,1.2));
#9577=CARTESIAN_POINT('Origin',(-6.5,18.2,1.2));
#9578=CARTESIAN_POINT('',(-6.5,18.2,1.2));
#9579=CARTESIAN_POINT('',(-6.5,18.2,3.2));
#9580=CARTESIAN_POINT('Origin',(0.,16.,3.2));
#9581=CARTESIAN_POINT('Origin',(0.,16.,1.2));
#9582=CARTESIAN_POINT('',(0.,0.,0.));
#9583=CARTESIAN_POINT('Origin',(-4.75,16.,3.2));
#9584=CARTESIAN_POINT('',(-5.175,16.,4.4));
#9585=CARTESIAN_POINT('Origin',(-4.75,16.,4.4));
#9586=CARTESIAN_POINT('',(-5.175,16.,3.2));
#9587=CARTESIAN_POINT('',(-5.175,16.,3.2));
#9588=CARTESIAN_POINT('Origin',(-4.75,16.,3.2));
#9589=CARTESIAN_POINT('Origin',(-4.75,16.,3.2));
#9590=CARTESIAN_POINT('',(-5.395,16.,4.4));
#9591=CARTESIAN_POINT('Origin',(-4.75,16.,4.4));
#9592=CARTESIAN_POINT('',(-5.395,16.,3.2));
#9593=CARTESIAN_POINT('',(-5.395,16.,3.2));
#9594=CARTESIAN_POINT('Origin',(-4.75,16.,3.2));
#9595=CARTESIAN_POINT('Origin',(-4.75,16.,4.4));
#9596=CARTESIAN_POINT('Origin',(-4.75,16.,3.2));
#9597=CARTESIAN_POINT('',(0.,0.,0.));
#9598=CARTESIAN_POINT('Origin',(4.75,16.,3.2));
#9599=CARTESIAN_POINT('',(4.325,16.,4.4));
#9600=CARTESIAN_POINT('Origin',(4.75,16.,4.4));
#9601=CARTESIAN_POINT('',(4.325,16.,3.2));
#9602=CARTESIAN_POINT('',(4.325,16.,3.2));
#9603=CARTESIAN_POINT('Origin',(4.75,16.,3.2));
#9604=CARTESIAN_POINT('Origin',(4.75,16.,3.2));
#9605=CARTESIAN_POINT('',(4.105,16.,4.4));
#9606=CARTESIAN_POINT('Origin',(4.75,16.,4.4));
#9607=CARTESIAN_POINT('',(4.105,16.,3.2));
#9608=CARTESIAN_POINT('',(4.105,16.,3.2));
#9609=CARTESIAN_POINT('Origin',(4.75,16.,3.2));
#9610=CARTESIAN_POINT('Origin',(4.75,16.,4.4));
#9611=CARTESIAN_POINT('Origin',(4.75,16.,3.2));
#9612=CARTESIAN_POINT('',(0.,0.,0.));
#9613=CARTESIAN_POINT('Origin',(8.,-5.9,1.1));
#9614=CARTESIAN_POINT('',(7.725,-5.9,1.2));
#9615=CARTESIAN_POINT('Origin',(8.,-5.9,1.2));
#9616=CARTESIAN_POINT('',(7.725,-5.9,2.));
#9617=CARTESIAN_POINT('',(7.725,-5.9,1.1));
#9618=CARTESIAN_POINT('Origin',(8.,-5.9,2.));
#9619=CARTESIAN_POINT('Origin',(5.6,-5.9,1.1));
#9620=CARTESIAN_POINT('',(5.325,-5.9,1.2));
#9621=CARTESIAN_POINT('Origin',(5.6,-5.9,1.2));
#9622=CARTESIAN_POINT('',(5.325,-5.9,2.));
#9623=CARTESIAN_POINT('',(5.325,-5.9,1.1));
#9624=CARTESIAN_POINT('Origin',(5.6,-5.9,2.));
#9625=CARTESIAN_POINT('Origin',(6.5,-5.3,10.));
#9626=CARTESIAN_POINT('',(6.195,-5.2,10.));
#9627=CARTESIAN_POINT('Origin',(6.5,-5.2,10.));
#9628=CARTESIAN_POINT('',(6.195,-4.4,10.));
#9629=CARTESIAN_POINT('',(6.195,-5.3,10.));
#9630=CARTESIAN_POINT('Origin',(6.5,-4.4,10.));
#9631=CARTESIAN_POINT('Origin',(5.,-6.5,2.));
#9632=CARTESIAN_POINT('',(8.6,-6.5,2.));
#9633=CARTESIAN_POINT('',(5.,-6.5,2.));
#9634=CARTESIAN_POINT('',(8.6,-6.5,2.));
#9635=CARTESIAN_POINT('',(8.6,-3.3,2.));
#9636=CARTESIAN_POINT('',(8.6,-6.5,2.));
#9637=CARTESIAN_POINT('',(5.,-3.3,2.));
#9638=CARTESIAN_POINT('',(8.6,-3.3,2.));
#9639=CARTESIAN_POINT('',(5.,-6.5,2.));
#9640=CARTESIAN_POINT('',(8.,-4.4,2.));
#9641=CARTESIAN_POINT('',(5.6,-4.4,2.));
#9642=CARTESIAN_POINT('',(6.5,-4.4,2.));
#9643=CARTESIAN_POINT('',(8.,-5.2,2.));
#9644=CARTESIAN_POINT('',(8.,-5.85,2.));
#9645=CARTESIAN_POINT('',(5.6,-5.2,2.));
#9646=CARTESIAN_POINT('',(5.3,-5.2,2.));
#9647=CARTESIAN_POINT('',(5.6,-5.45,2.));
#9648=CARTESIAN_POINT('Origin',(5.,-6.5,1.2));
#9649=CARTESIAN_POINT('',(5.,-6.5,1.2));
#9650=CARTESIAN_POINT('',(5.,-6.5,2.));
#9651=CARTESIAN_POINT('',(5.,-3.3,1.2));
#9652=CARTESIAN_POINT('',(5.,-3.3,2.));
#9653=CARTESIAN_POINT('',(5.,-6.5,1.2));
#9654=CARTESIAN_POINT('Origin',(8.6,-6.5,2.));
#9655=CARTESIAN_POINT('',(8.6,-6.5,1.2));
#9656=CARTESIAN_POINT('',(8.6,-6.5,1.2));
#9657=CARTESIAN_POINT('',(8.6,-3.3,1.2));
#9658=CARTESIAN_POINT('',(8.6,-6.5,1.2));
#9659=CARTESIAN_POINT('',(8.6,-3.3,1.2));
#9660=CARTESIAN_POINT('Origin',(6.8,-3.3,1.6));
#9661=CARTESIAN_POINT('',(5.,-3.3,1.2));
#9662=CARTESIAN_POINT('Origin',(6.8,-6.5,1.6));
#9663=CARTESIAN_POINT('',(5.,-6.5,1.2));
#9664=CARTESIAN_POINT('Origin',(5.6,-5.2,1.2));
#9665=CARTESIAN_POINT('',(8.,-5.2,11.1));
#9666=CARTESIAN_POINT('',(8.,-5.2,1.2));
#9667=CARTESIAN_POINT('',(5.6,-5.2,11.1));
#9668=CARTESIAN_POINT('',(5.6,-5.2,11.1));
#9669=CARTESIAN_POINT('',(5.6,-5.2,1.2));
#9670=CARTESIAN_POINT('Origin',(8.,-5.2,1.2));
#9671=CARTESIAN_POINT('',(8.,-4.4,11.1));
#9672=CARTESIAN_POINT('',(8.,-4.4,1.2));
#9673=CARTESIAN_POINT('',(8.,-5.2,11.1));
#9674=CARTESIAN_POINT('Origin',(8.,-4.4,1.2));
#9675=CARTESIAN_POINT('',(5.6,-4.4,11.1));
#9676=CARTESIAN_POINT('',(5.6,-4.4,1.2));
#9677=CARTESIAN_POINT('',(8.,-4.4,11.1));
#9678=CARTESIAN_POINT('Origin',(5.6,-4.4,1.2));
#9679=CARTESIAN_POINT('',(5.6,-4.4,11.1));
#9680=CARTESIAN_POINT('Origin',(6.8,-4.8,11.1));
#9681=CARTESIAN_POINT('Origin',(6.8,-4.8,1.2));
#9682=CARTESIAN_POINT('',(0.,0.,0.));
#9683=CARTESIAN_POINT('Origin',(6.5,-3.8,10.));
#9684=CARTESIAN_POINT('',(6.335,-3.8,10.));
#9685=CARTESIAN_POINT('Origin',(6.5,-3.8,10.));
#9686=CARTESIAN_POINT('',(6.335,-2.9,10.));
#9687=CARTESIAN_POINT('',(6.335,-3.8,10.));
#9688=CARTESIAN_POINT('Origin',(6.5,-2.9,10.));
#9689=CARTESIAN_POINT('Origin',(6.5,-3.8,10.));
#9690=CARTESIAN_POINT('Origin',(6.5,-5.2,10.));
#9691=CARTESIAN_POINT('',(5.9,-5.2,10.));
#9692=CARTESIAN_POINT('Origin',(6.5,-5.2,10.));
#9693=CARTESIAN_POINT('',(6.2,-5.2,10.));
#9694=CARTESIAN_POINT('Origin',(6.5,-5.2,10.));
#9695=CARTESIAN_POINT('Origin',(6.5,-5.5,10.));
#9696=CARTESIAN_POINT('',(5.9,-5.5,10.));
#9697=CARTESIAN_POINT('',(5.9,-5.5,10.));
#9698=CARTESIAN_POINT('Origin',(6.5,-5.5,10.));
#9699=CARTESIAN_POINT('Origin',(6.5,-5.5,10.));
#9700=CARTESIAN_POINT('Origin',(6.5,-5.2,10.));
#9701=CARTESIAN_POINT('',(6.2,-2.9,10.));
#9702=CARTESIAN_POINT('Origin',(6.5,-2.9,10.));
#9703=CARTESIAN_POINT('',(6.2,-5.2,10.));
#9704=CARTESIAN_POINT('Origin',(6.5,-2.9,10.));
#9705=CARTESIAN_POINT('',(0.,0.,0.));
#9706=CARTESIAN_POINT('Origin',(6.5,-4.4,10.));
#9707=CARTESIAN_POINT('',(6.195,-3.5,10.));
#9708=CARTESIAN_POINT('Origin',(6.5,-3.5,10.));
#9709=CARTESIAN_POINT('',(6.195,-4.4,10.));
#9710=CARTESIAN_POINT('',(6.195,-4.4,10.));
#9711=CARTESIAN_POINT('Origin',(6.5,-4.4,10.));
#9712=CARTESIAN_POINT('Origin',(6.5,-4.4,10.));
#9713=CARTESIAN_POINT('',(6.,-3.5,10.));
#9714=CARTESIAN_POINT('Origin',(6.5,-3.5,10.));
#9715=CARTESIAN_POINT('',(6.,-4.4,10.));
#9716=CARTESIAN_POINT('',(6.,-4.4,10.));
#9717=CARTESIAN_POINT('Origin',(6.5,-4.4,10.));
#9718=CARTESIAN_POINT('Origin',(6.5,-3.5,10.));
#9719=CARTESIAN_POINT('Origin',(6.5,-4.4,10.));
#9720=CARTESIAN_POINT('',(0.,0.,0.));
#9721=CARTESIAN_POINT('Origin',(6.5,-2.9,10.));
#9722=CARTESIAN_POINT('',(6.275,-2.7,10.));
#9723=CARTESIAN_POINT('Origin',(6.5,-2.7,10.));
#9724=CARTESIAN_POINT('',(6.275,-2.9,10.));
#9725=CARTESIAN_POINT('',(6.275,-2.9,10.));
#9726=CARTESIAN_POINT('Origin',(6.5,-2.9,10.));
#9727=CARTESIAN_POINT('Origin',(6.5,-2.9,10.));
#9728=CARTESIAN_POINT('',(5.9,-2.7,10.));
#9729=CARTESIAN_POINT('Origin',(6.5,-2.7,10.));
#9730=CARTESIAN_POINT('',(5.9,-2.9,10.));
#9731=CARTESIAN_POINT('',(5.9,-2.9,10.));
#9732=CARTESIAN_POINT('Origin',(6.5,-2.9,10.));
#9733=CARTESIAN_POINT('Origin',(6.5,-2.7,10.));
#9734=CARTESIAN_POINT('Origin',(6.5,-2.9,10.));
#9735=CARTESIAN_POINT('',(0.,0.,0.));
#9736=CARTESIAN_POINT('Origin',(7.9,-3.4,6.5));
#9737=CARTESIAN_POINT('',(6.76547231270358,-3.4,9.3));
#9738=CARTESIAN_POINT('',(7.9,-3.4,6.5));
#9739=CARTESIAN_POINT('',(6.76547231270358,-3.4,9.3));
#9740=CARTESIAN_POINT('',(6.76547231270358,-3.,9.3));
#9741=CARTESIAN_POINT('',(6.76547231270358,-3.4,9.3));
#9742=CARTESIAN_POINT('',(7.9,-3.,6.5));
#9743=CARTESIAN_POINT('',(6.76547231270358,-3.,9.3));
#9744=CARTESIAN_POINT('',(7.9,-3.4,6.5));
#9745=CARTESIAN_POINT('Origin',(7.98,-3.4,6.5));
#9746=CARTESIAN_POINT('',(7.98,-3.4,6.5));
#9747=CARTESIAN_POINT('',(7.9,-3.4,6.5));
#9748=CARTESIAN_POINT('',(7.98,-3.,6.5));
#9749=CARTESIAN_POINT('',(7.9,-3.,6.5));
#9750=CARTESIAN_POINT('',(7.98,-3.4,6.5));
#9751=CARTESIAN_POINT('Origin',(6.84547231270358,-3.4,9.3));
#9752=CARTESIAN_POINT('',(6.84547231270358,-3.4,9.3));
#9753=CARTESIAN_POINT('',(7.98,-3.4,6.5));
#9754=CARTESIAN_POINT('',(6.84547231270358,-3.,9.3));
#9755=CARTESIAN_POINT('',(7.98,-3.,6.5));
#9756=CARTESIAN_POINT('',(6.84547231270358,-3.4,9.3));
#9757=CARTESIAN_POINT('Origin',(6.76547231270358,-3.4,9.3));
#9758=CARTESIAN_POINT('',(6.84547231270358,-3.4,9.3));
#9759=CARTESIAN_POINT('',(6.84547231270358,-3.,9.3));
#9760=CARTESIAN_POINT('Origin',(7.37273615635179,-3.,7.9));
#9761=CARTESIAN_POINT('Origin',(7.37273615635179,-3.4,7.9));
#9762=CARTESIAN_POINT('',(0.,0.,0.));
#9763=CARTESIAN_POINT('Origin',(8.3,-3.7,5.4));
#9764=CARTESIAN_POINT('',(8.135,-3.7,5.5));
#9765=CARTESIAN_POINT('Origin',(8.3,-3.7,5.5));
#9766=CARTESIAN_POINT('',(8.135,-3.7,6.5));
#9767=CARTESIAN_POINT('',(8.135,-3.7,5.4));
#9768=CARTESIAN_POINT('Origin',(8.3,-3.7,6.5));
#9769=CARTESIAN_POINT('Origin',(8.7,-3.,5.5));
#9770=CARTESIAN_POINT('',(8.7,-3.,5.5));
#9771=CARTESIAN_POINT('',(7.9,-3.,5.5));
#9772=CARTESIAN_POINT('',(8.7,-3.,5.5));
#9773=CARTESIAN_POINT('',(7.9,-3.,6.5));
#9774=CARTESIAN_POINT('',(7.9,-3.,5.5));
#9775=CARTESIAN_POINT('',(8.7,-3.,6.5));
#9776=CARTESIAN_POINT('',(8.7,-3.,6.5));
#9777=CARTESIAN_POINT('',(8.7,-3.,5.5));
#9778=CARTESIAN_POINT('Origin',(8.7,-4.4,5.5));
#9779=CARTESIAN_POINT('',(8.7,-4.4,5.5));
#9780=CARTESIAN_POINT('',(8.7,-4.4,5.5));
#9781=CARTESIAN_POINT('',(8.7,-4.4,6.5));
#9782=CARTESIAN_POINT('',(8.7,-4.4,6.5));
#9783=CARTESIAN_POINT('',(8.7,-4.4,5.5));
#9784=CARTESIAN_POINT('Origin',(7.9,-4.4,5.5));
#9785=CARTESIAN_POINT('',(7.9,-4.4,5.5));
#9786=CARTESIAN_POINT('',(7.9,-4.4,5.5));
#9787=CARTESIAN_POINT('',(7.9,-4.4,6.5));
#9788=CARTESIAN_POINT('',(7.9,-4.4,6.5));
#9789=CARTESIAN_POINT('',(7.9,-4.4,5.5));
#9790=CARTESIAN_POINT('Origin',(7.9,-3.,5.5));
#9791=CARTESIAN_POINT('',(7.9,-3.,5.5));
#9792=CARTESIAN_POINT('',(7.9,-3.,6.5));
#9793=CARTESIAN_POINT('Origin',(8.3,-3.7,6.5));
#9794=CARTESIAN_POINT('Origin',(8.3,-3.7,5.5));
#9795=CARTESIAN_POINT('',(0.,0.,0.));
#9796=CARTESIAN_POINT('',(0.,0.,0.));
#9797=CARTESIAN_POINT('Origin',(0.,0.,0.));
#9798=CARTESIAN_POINT('',(-2.05,-1.65,2.51052593825207E-16));
#9799=CARTESIAN_POINT('Origin',(0.,-1.65,0.));
#9800=CARTESIAN_POINT('',(-2.05,-1.14891252930761,-2.51052593825207E-16));
#9801=CARTESIAN_POINT('',(-2.05,0.,2.51052593825207E-16));
#9802=CARTESIAN_POINT('Origin',(0.,-1.14891252930761,0.));
#9803=CARTESIAN_POINT('Origin',(0.,0.,0.));
#9804=CARTESIAN_POINT('',(-2.05,1.14891252930761,2.51052593825207E-16));
#9805=CARTESIAN_POINT('Origin',(0.,1.14891252930761,0.));
#9806=CARTESIAN_POINT('',(-2.05,1.65,-2.51052593825207E-16));
#9807=CARTESIAN_POINT('',(-2.05,0.,2.51052593825207E-16));
#9808=CARTESIAN_POINT('Origin',(0.,1.65,0.));
#9809=CARTESIAN_POINT('Origin',(0.,0.,0.));
#9810=CARTESIAN_POINT('',(-1.43895998899814E-16,-1.76221774462768E-32,-2.35));
#9811=CARTESIAN_POINT('',(-1.43895998899814E-16,-1.76221774462768E-32,2.35));
#9812=CARTESIAN_POINT('Origin',(0.,0.,0.));
#9813=CARTESIAN_POINT('Origin',(0.,1.55,-1.49));
#9814=CARTESIAN_POINT('',(-3.76384615384615,1.55,-2.13));
#9815=CARTESIAN_POINT('',(-1.81744325908679,1.55,-2.13));
#9816=CARTESIAN_POINT('',(0.,1.55,-2.13));
#9817=CARTESIAN_POINT('',(-2.46585583768694,1.55,-1.32648218523477));
#9818=CARTESIAN_POINT('',(-1.68,1.55,-0.84));
#9819=CARTESIAN_POINT('Origin',(0.,1.55,0.));
#9820=CARTESIAN_POINT('Origin',(0.,1.55,-1.49));
#9821=CARTESIAN_POINT('',(1.81744325908679,1.55,-2.13));
#9822=CARTESIAN_POINT('',(3.76384615384615,1.55,-2.13));
#9823=CARTESIAN_POINT('',(0.,1.55,-2.13));
#9824=CARTESIAN_POINT('',(2.46585583768694,1.55,-1.32648218523477));
#9825=CARTESIAN_POINT('Origin',(0.,1.55,0.));
#9826=CARTESIAN_POINT('',(3.78,1.55,-2.14));
#9827=CARTESIAN_POINT('Origin',(0.,-1.55,-1.49));
#9828=CARTESIAN_POINT('',(-1.81744325908679,-1.55,-2.13));
#9829=CARTESIAN_POINT('',(-3.76384615384615,-1.55,-2.13));
#9830=CARTESIAN_POINT('',(0.,-1.55,-2.13));
#9831=CARTESIAN_POINT('',(-2.46585583768694,-1.55,-1.32648218523477));
#9832=CARTESIAN_POINT('Origin',(0.,-1.55,0.));
#9833=CARTESIAN_POINT('',(-1.68,-1.55,-0.84));
#9834=CARTESIAN_POINT('Origin',(-3.78,0.,-2.14));
#9835=CARTESIAN_POINT('',(-3.76384615384615,0.,-2.13));
#9836=CARTESIAN_POINT('',(-2.46585583768694,0.,-1.32648218523477));
#9837=CARTESIAN_POINT('Origin',(0.,-1.55,-1.49));
#9838=CARTESIAN_POINT('',(3.76384615384615,-1.55,-2.13));
#9839=CARTESIAN_POINT('',(1.81744325908679,-1.55,-2.13));
#9840=CARTESIAN_POINT('',(0.,-1.55,-2.13));
#9841=CARTESIAN_POINT('',(2.46585583768694,-1.55,-1.32648218523477));
#9842=CARTESIAN_POINT('',(3.78,-1.55,-2.14));
#9843=CARTESIAN_POINT('Origin',(0.,-1.55,0.));
#9844=CARTESIAN_POINT('Origin',(1.68,0.,-0.84));
#9845=CARTESIAN_POINT('',(3.76384615384615,0.,-2.13));
#9846=CARTESIAN_POINT('',(2.46585583768694,0.,-1.32648218523477));
#9847=CARTESIAN_POINT('Origin',(0.,0.,-2.13));
#9848=CARTESIAN_POINT('',(-6.35,1.9,-2.13));
#9849=CARTESIAN_POINT('',(-6.35,-1.9,-2.13));
#9850=CARTESIAN_POINT('',(-6.35,1.9,-2.13));
#9851=CARTESIAN_POINT('',(6.35,-1.9,-2.13));
#9852=CARTESIAN_POINT('',(-6.35,-1.9,-2.13));
#9853=CARTESIAN_POINT('',(6.35,1.9,-2.13));
#9854=CARTESIAN_POINT('',(6.35,-1.9,-2.13));
#9855=CARTESIAN_POINT('',(6.35,1.9,-2.13));
#9856=CARTESIAN_POINT('',(4.1,7.9602041944578E-17,-2.13));
#9857=CARTESIAN_POINT('Origin',(4.75,0.,-2.13));
#9858=CARTESIAN_POINT('',(-5.4,7.9602041944578E-17,-2.13));
#9859=CARTESIAN_POINT('Origin',(-4.75,0.,-2.13));
#9860=CARTESIAN_POINT('',(1.81744325908679,-1.65,-2.13));
#9861=CARTESIAN_POINT('',(1.81744325908679,0.,-2.13));
#9862=CARTESIAN_POINT('',(-1.81744325908679,-1.65,-2.13));
#9863=CARTESIAN_POINT('',(0.,-1.65,-2.13));
#9864=CARTESIAN_POINT('',(-1.81744325908679,0.,-2.13));
#9865=CARTESIAN_POINT('',(-1.81744325908679,1.65,-2.13));
#9866=CARTESIAN_POINT('',(-1.81744325908679,0.,-2.13));
#9867=CARTESIAN_POINT('',(1.81744325908679,1.65,-2.13));
#9868=CARTESIAN_POINT('',(0.,1.65,-2.13));
#9869=CARTESIAN_POINT('',(1.81744325908679,0.,-2.13));
#9870=CARTESIAN_POINT('Origin',(0.,0.,0.));
#9871=CARTESIAN_POINT('Origin',(0.,1.65,0.));
#9872=CARTESIAN_POINT('Origin',(0.,-1.65,0.));
#9873=CARTESIAN_POINT('Origin',(0.,-1.65,0.));
#9874=CARTESIAN_POINT('Origin',(0.,1.65,0.));
#9875=CARTESIAN_POINT('Origin',(3.35,1.4,-3.33));
#9876=CARTESIAN_POINT('',(3.35,1.4,-3.33));
#9877=CARTESIAN_POINT('',(-3.35,1.4,-3.33));
#9878=CARTESIAN_POINT('',(1.675,1.4,-3.33));
#9879=CARTESIAN_POINT('',(3.35,1.4,-2.83));
#9880=CARTESIAN_POINT('',(3.35,1.4,-3.33));
#9881=CARTESIAN_POINT('',(-3.35,1.4,-2.83));
#9882=CARTESIAN_POINT('',(3.35,1.4,-2.83));
#9883=CARTESIAN_POINT('',(-3.35,1.4,-3.33));
#9884=CARTESIAN_POINT('Origin',(3.35,-1.4,-3.33));
#9885=CARTESIAN_POINT('',(3.35,-1.4,-3.33));
#9886=CARTESIAN_POINT('',(3.35,-0.7,-3.33));
#9887=CARTESIAN_POINT('',(3.35,-1.4,-2.83));
#9888=CARTESIAN_POINT('',(3.35,-1.4,-3.33));
#9889=CARTESIAN_POINT('',(3.35,-1.4,-2.83));
#9890=CARTESIAN_POINT('Origin',(-3.35,-1.4,-3.33));
#9891=CARTESIAN_POINT('',(-3.35,-1.4,-3.33));
#9892=CARTESIAN_POINT('',(-1.675,-1.4,-3.33));
#9893=CARTESIAN_POINT('',(-3.35,-1.4,-2.83));
#9894=CARTESIAN_POINT('',(-3.35,-1.4,-3.33));
#9895=CARTESIAN_POINT('',(-3.35,-1.4,-2.83));
#9896=CARTESIAN_POINT('Origin',(-3.35,1.4,-3.33));
#9897=CARTESIAN_POINT('',(-3.35,0.7,-3.33));
#9898=CARTESIAN_POINT('',(-3.35,1.4,-2.83));
#9899=CARTESIAN_POINT('Origin',(0.,0.,-2.83));
#9900=CARTESIAN_POINT('Origin',(-4.75,0.,-3.33));
#9901=CARTESIAN_POINT('',(-5.4,-7.9602041944578E-17,-3.33));
#9902=CARTESIAN_POINT('Origin',(-4.75,0.,-3.33));
#9903=CARTESIAN_POINT('',(-5.4,-7.9602041944578E-17,-3.33));
#9904=CARTESIAN_POINT('Origin',(4.75,0.,-3.33));
#9905=CARTESIAN_POINT('',(4.1,-7.9602041944578E-17,-3.33));
#9906=CARTESIAN_POINT('Origin',(4.75,0.,-3.33));
#9907=CARTESIAN_POINT('',(4.1,-7.9602041944578E-17,-3.33));
#9908=CARTESIAN_POINT('Origin',(6.35,1.9,-3.33));
#9909=CARTESIAN_POINT('',(6.35,1.9,-3.33));
#9910=CARTESIAN_POINT('',(-6.35,1.9,-3.33));
#9911=CARTESIAN_POINT('',(6.35,1.9,-3.33));
#9912=CARTESIAN_POINT('',(-6.35,1.9,-3.33));
#9913=CARTESIAN_POINT('',(6.35,1.9,-3.33));
#9914=CARTESIAN_POINT('Origin',(6.35,-1.9,-3.33));
#9915=CARTESIAN_POINT('',(6.35,-1.9,-3.33));
#9916=CARTESIAN_POINT('',(6.35,-1.9,-3.33));
#9917=CARTESIAN_POINT('',(6.35,-1.9,-3.33));
#9918=CARTESIAN_POINT('Origin',(-6.35,-1.9,-3.33));
#9919=CARTESIAN_POINT('',(-6.35,-1.9,-3.33));
#9920=CARTESIAN_POINT('',(-6.35,-1.9,-3.33));
#9921=CARTESIAN_POINT('',(-6.35,-1.9,-3.33));
#9922=CARTESIAN_POINT('Origin',(-6.35,1.9,-3.33));
#9923=CARTESIAN_POINT('',(-6.35,1.9,-3.33));
#9924=CARTESIAN_POINT('Origin',(0.,0.,-3.33));
#9925=CARTESIAN_POINT('',(0.,0.,0.));
#9926=CARTESIAN_POINT('Origin',(0.,0.,0.));
#9927=CARTESIAN_POINT('',(-1.8,-0.85,-2.20436423846524E-16));
#9928=CARTESIAN_POINT('Origin',(0.,-0.85,0.));
#9929=CARTESIAN_POINT('',(-1.8,0.85,-2.20436423846524E-16));
#9930=CARTESIAN_POINT('',(-1.8,0.,-2.20436423846524E-16));
#9931=CARTESIAN_POINT('Origin',(0.,0.85,0.));
#9932=CARTESIAN_POINT('Origin',(2.19089023002066,0.85,0.));
#9933=CARTESIAN_POINT('',(2.19089023002066,0.85,0.));
#9934=CARTESIAN_POINT('Origin',(0.,0.85,0.));
#9935=CARTESIAN_POINT('Origin',(3.99680288865056E-15,0.,0.));
#9936=CARTESIAN_POINT('',(3.85290688975075E-15,-1.76221774462768E-32,2.35));
#9937=CARTESIAN_POINT('',(3.85290688975075E-15,-1.76221774462768E-32,-2.35));
#9938=CARTESIAN_POINT('Origin',(3.99680288865056E-15,0.,0.));
#9939=CARTESIAN_POINT('',(2.19089023002066,-0.85,0.));
#9940=CARTESIAN_POINT('Origin',(0.,-0.85,0.));
#9941=CARTESIAN_POINT('Origin',(1.8,-0.85,0.));
#9942=CARTESIAN_POINT('Origin',(0.,1.55,0.));
#9943=CARTESIAN_POINT('',(1.42894191624432,1.8,0.825000000000001));
#9944=CARTESIAN_POINT('',(1.53744468918255,1.55,0.598968970568896));
#9945=CARTESIAN_POINT('Ctrl Pts',(1.42894191624432,1.8,0.825000000000001));
#9946=CARTESIAN_POINT('Ctrl Pts',(1.44466308895875,1.8,0.797770130104052));
#9947=CARTESIAN_POINT('Ctrl Pts',(1.46055812562105,1.79370633789704,0.768258557763732));
#9948=CARTESIAN_POINT('Ctrl Pts',(1.48824888379079,1.76817777258318,0.713138492740816));
#9949=CARTESIAN_POINT('Ctrl Pts',(1.50008999307766,1.74894552961493,0.687551581002689));
#9950=CARTESIAN_POINT('Ctrl Pts',(1.51812136280714,1.70460745840382,0.646764802471699));
#9951=CARTESIAN_POINT('Ctrl Pts',(1.52552758004446,1.67652816181843,0.628833667319578));
#9952=CARTESIAN_POINT('Ctrl Pts',(1.53516661651472,1.61494799959182,0.604921184808251));
#9953=CARTESIAN_POINT('Ctrl Pts',(1.53744468918255,1.58144291640553,0.598968970568896));
#9954=CARTESIAN_POINT('Ctrl Pts',(1.53744468918255,1.55,0.598968970568896));
#9955=CARTESIAN_POINT('',(1.42894191624432,1.3,0.825000000000001));
#9956=CARTESIAN_POINT('Ctrl Pts',(1.42894191624432,1.3,0.825000000000001));
#9957=CARTESIAN_POINT('Ctrl Pts',(1.4132207435299,1.3,0.852229869895949));
#9958=CARTESIAN_POINT('Ctrl Pts',(1.39561049050871,1.30629366210296,0.880751161609749));
#9959=CARTESIAN_POINT('Ctrl Pts',(1.36172049302549,1.33182222741682,0.932292094146256));
#9960=CARTESIAN_POINT('Ctrl Pts',(1.34548213209931,1.35105447038507,0.955340251466734));
#9961=CARTESIAN_POINT('Ctrl Pts',(1.31917543061769,1.39539254159618,0.99134926498299));
#9962=CARTESIAN_POINT('Ctrl Pts',(1.30734972067592,1.42347183818157,1.00672880483252));
#9963=CARTESIAN_POINT('Ctrl Pts',(1.29146042158868,1.48505200040818,1.02703269653942));
#9964=CARTESIAN_POINT('Ctrl Pts',(1.28744468918255,1.51855708359447,1.03198167246111));
#9965=CARTESIAN_POINT('Ctrl Pts',(1.28744468918255,1.58144291640553,1.03198167246111));
#9966=CARTESIAN_POINT('Ctrl Pts',(1.29146042158868,1.61494799959182,1.02703269653942));
#9967=CARTESIAN_POINT('Ctrl Pts',(1.30734972067592,1.67652816181843,1.00672880483252));
#9968=CARTESIAN_POINT('Ctrl Pts',(1.31917543061769,1.70460745840382,0.991349264982991));
#9969=CARTESIAN_POINT('Ctrl Pts',(1.34548213209931,1.74894552961493,0.955340251466735));
#9970=CARTESIAN_POINT('Ctrl Pts',(1.36172049302549,1.76817777258318,0.932292094146256));
#9971=CARTESIAN_POINT('Ctrl Pts',(1.39561049050871,1.79370633789704,0.880751161609749));
#9972=CARTESIAN_POINT('Ctrl Pts',(1.4132207435299,1.8,0.85222986989595));
#9973=CARTESIAN_POINT('Ctrl Pts',(1.42894191624432,1.8,0.825000000000001));
#9974=CARTESIAN_POINT('Ctrl Pts',(1.53744468918255,1.55,0.598968970568896));
#9975=CARTESIAN_POINT('Ctrl Pts',(1.53744468918255,1.51855708359447,0.598968970568896));
#9976=CARTESIAN_POINT('Ctrl Pts',(1.53516661651472,1.48505200040818,0.60492118480825));
#9977=CARTESIAN_POINT('Ctrl Pts',(1.52552758004446,1.42347183818157,0.628833667319578));
#9978=CARTESIAN_POINT('Ctrl Pts',(1.51812136280714,1.39539254159618,0.646764802471699));
#9979=CARTESIAN_POINT('Ctrl Pts',(1.50008999307766,1.35105447038507,0.687551581002689));
#9980=CARTESIAN_POINT('Ctrl Pts',(1.48824888379079,1.33182222741682,0.713138492740816));
#9981=CARTESIAN_POINT('Ctrl Pts',(1.46055812562105,1.30629366210296,0.768258557763732));
#9982=CARTESIAN_POINT('Ctrl Pts',(1.44466308895875,1.3,0.797770130104052));
#9983=CARTESIAN_POINT('Ctrl Pts',(1.42894191624432,1.3,0.825000000000001));
#9984=CARTESIAN_POINT('',(0.963525491562421,1.55,0.267616567329818));
#9985=CARTESIAN_POINT('',(0.125,1.55,-0.21650635094611));
#9986=CARTESIAN_POINT('Ctrl Pts',(0.963525491562421,1.55,0.267616567329818));
#9987=CARTESIAN_POINT('Ctrl Pts',(0.963525491562421,1.5815373526696,0.267616567329818));
#9988=CARTESIAN_POINT('Ctrl Pts',(0.961833761492987,1.61508042700263,0.273949373987484));
#9989=CARTESIAN_POINT('Ctrl Pts',(0.954308486908894,1.67663267125761,0.299111603474268));
#9990=CARTESIAN_POINT('Ctrl Pts',(0.948394987258249,1.70465411363682,0.31788699900678));
#9991=CARTESIAN_POINT('Ctrl Pts',(0.933155485613026,1.74889618382539,0.360174810895352));
#9992=CARTESIAN_POINT('Ctrl Pts',(0.92278792026947,1.76811531482682,0.386546956384144));
#9993=CARTESIAN_POINT('Ctrl Pts',(0.897143218189782,1.79367084275751,0.442820664919227));
#9994=CARTESIAN_POINT('Ctrl Pts',(0.881791875377343,1.8,0.472691670144998));
#9995=CARTESIAN_POINT('Ctrl Pts',(0.850258932191534,1.8,0.527308329855003));
#9996=CARTESIAN_POINT('Ctrl Pts',(0.832065554235658,1.79367084275751,0.555538485325664));
#9997=CARTESIAN_POINT('Ctrl Pts',(0.796153444118959,1.76811531482682,0.605884303066698));
#9998=CARTESIAN_POINT('Ctrl Pts',(0.778498278845144,1.74889618382539,0.62804895077401));
#9999=CARTESIAN_POINT('Ctrl Pts',(0.749495710301794,1.70465411363682,0.662390652284073));
#10000=CARTESIAN_POINT('Ctrl Pts',(0.73619249062986,1.67663267125761,0.676899590973058));
#10001=CARTESIAN_POINT('Ctrl Pts',(0.718163997970498,1.61508042700263,0.695997784676728));
#10002=CARTESIAN_POINT('Ctrl Pts',(0.713525491562421,1.5815373526696,0.700629269222037));
#10003=CARTESIAN_POINT('Ctrl Pts',(0.713525491562421,1.5184626473304,0.700629269222037));
#10004=CARTESIAN_POINT('Ctrl Pts',(0.718163997970498,1.48491957299737,0.695997784676728));
#10005=CARTESIAN_POINT('Ctrl Pts',(0.73619249062986,1.42336732874239,0.676899590973058));
#10006=CARTESIAN_POINT('Ctrl Pts',(0.749495710301794,1.39534588636318,0.662390652284073));
#10007=CARTESIAN_POINT('Ctrl Pts',(0.778498278845144,1.35110381617461,0.62804895077401));
#10008=CARTESIAN_POINT('Ctrl Pts',(0.796153444118959,1.33188468517318,0.605884303066698));
#10009=CARTESIAN_POINT('Ctrl Pts',(0.832065554235658,1.30632915724249,0.555538485325664));
#10010=CARTESIAN_POINT('Ctrl Pts',(0.850258932191534,1.3,0.527308329855003));
#10011=CARTESIAN_POINT('Ctrl Pts',(0.881791875377343,1.3,0.472691670144998));
#10012=CARTESIAN_POINT('Ctrl Pts',(0.897143218189782,1.30632915724249,0.442820664919227));
#10013=CARTESIAN_POINT('Ctrl Pts',(0.92278792026947,1.33188468517318,0.386546956384144));
#10014=CARTESIAN_POINT('Ctrl Pts',(0.933155485613026,1.35110381617461,0.360174810895352));
#10015=CARTESIAN_POINT('Ctrl Pts',(0.948394987258249,1.39534588636318,0.31788699900678));
#10016=CARTESIAN_POINT('Ctrl Pts',(0.954308486908894,1.42336732874239,0.299111603474268));
#10017=CARTESIAN_POINT('Ctrl Pts',(0.961833761492987,1.48491957299738,0.273949373987484));
#10018=CARTESIAN_POINT('Ctrl Pts',(0.963525491562421,1.5184626473304,0.267616567329818));
#10019=CARTESIAN_POINT('Ctrl Pts',(0.963525491562421,1.55,0.267616567329818));
#10020=CARTESIAN_POINT('Origin',(0.,1.55,0.));
#10021=CARTESIAN_POINT('',(-0.713525491562421,1.55,-0.700629269222037));
#10022=CARTESIAN_POINT('Ctrl Pts',(-0.713525491562421,1.55,-0.700629269222037));
#10023=CARTESIAN_POINT('Ctrl Pts',(-0.713525491562421,1.5184626473304,-0.700629269222037));
#10024=CARTESIAN_POINT('Ctrl Pts',(-0.718163997970498,1.48491957299737,
-0.695997784676728));
#10025=CARTESIAN_POINT('Ctrl Pts',(-0.73619249062986,1.42336732874239,-0.676899590973058));
#10026=CARTESIAN_POINT('Ctrl Pts',(-0.749495710301794,1.39534588636318,
-0.662390652284073));
#10027=CARTESIAN_POINT('Ctrl Pts',(-0.778498278845144,1.35110381617461,
-0.62804895077401));
#10028=CARTESIAN_POINT('Ctrl Pts',(-0.796153444118959,1.33188468517318,
-0.605884303066698));
#10029=CARTESIAN_POINT('Ctrl Pts',(-0.832065554235658,1.30632915724249,
-0.555538485325664));
#10030=CARTESIAN_POINT('Ctrl Pts',(-0.850258932191534,1.3,-0.527308329855003));
#10031=CARTESIAN_POINT('Ctrl Pts',(-0.881791875377343,1.3,-0.472691670144998));
#10032=CARTESIAN_POINT('Ctrl Pts',(-0.897143218189782,1.30632915724249,
-0.442820664919227));
#10033=CARTESIAN_POINT('Ctrl Pts',(-0.92278792026947,1.33188468517318,-0.386546956384144));
#10034=CARTESIAN_POINT('Ctrl Pts',(-0.933155485613026,1.35110381617461,
-0.360174810895352));
#10035=CARTESIAN_POINT('Ctrl Pts',(-0.948394987258249,1.39534588636318,
-0.31788699900678));
#10036=CARTESIAN_POINT('Ctrl Pts',(-0.954308486908894,1.42336732874239,
-0.299111603474268));
#10037=CARTESIAN_POINT('Ctrl Pts',(-0.961833761492986,1.48491957299737,
-0.273949373987484));
#10038=CARTESIAN_POINT('Ctrl Pts',(-0.963525491562421,1.5184626473304,-0.267616567329818));
#10039=CARTESIAN_POINT('Ctrl Pts',(-0.963525491562421,1.5815373526696,-0.267616567329818));
#10040=CARTESIAN_POINT('Ctrl Pts',(-0.961833761492986,1.61508042700263,
-0.273949373987484));
#10041=CARTESIAN_POINT('Ctrl Pts',(-0.954308486908894,1.67663267125761,
-0.299111603474268));
#10042=CARTESIAN_POINT('Ctrl Pts',(-0.948394987258249,1.70465411363682,
-0.31788699900678));
#10043=CARTESIAN_POINT('Ctrl Pts',(-0.933155485613026,1.74889618382539,
-0.360174810895352));
#10044=CARTESIAN_POINT('Ctrl Pts',(-0.92278792026947,1.76811531482682,-0.386546956384144));
#10045=CARTESIAN_POINT('Ctrl Pts',(-0.897143218189782,1.79367084275751,
-0.442820664919227));
#10046=CARTESIAN_POINT('Ctrl Pts',(-0.881791875377343,1.8,-0.472691670144998));
#10047=CARTESIAN_POINT('Ctrl Pts',(-0.850258932191534,1.8,-0.527308329855003));
#10048=CARTESIAN_POINT('Ctrl Pts',(-0.832065554235658,1.79367084275751,
-0.555538485325664));
#10049=CARTESIAN_POINT('Ctrl Pts',(-0.796153444118959,1.76811531482682,
-0.605884303066698));
#10050=CARTESIAN_POINT('Ctrl Pts',(-0.778498278845144,1.74889618382539,
-0.62804895077401));
#10051=CARTESIAN_POINT('Ctrl Pts',(-0.749495710301794,1.70465411363682,
-0.662390652284073));
#10052=CARTESIAN_POINT('Ctrl Pts',(-0.73619249062986,1.67663267125761,-0.676899590973058));
#10053=CARTESIAN_POINT('Ctrl Pts',(-0.718163997970498,1.61508042700263,
-0.695997784676728));
#10054=CARTESIAN_POINT('Ctrl Pts',(-0.713525491562421,1.5815373526696,-0.700629269222037));
#10055=CARTESIAN_POINT('Ctrl Pts',(-0.713525491562421,1.55,-0.700629269222037));
#10056=CARTESIAN_POINT('',(-1.28744468918255,1.55,-1.03198167246111));
#10057=CARTESIAN_POINT('',(0.125,1.55,-0.21650635094611));
#10058=CARTESIAN_POINT('',(-1.42894191624432,1.3,-0.825000000000001));
#10059=CARTESIAN_POINT('Ctrl Pts',(-1.42894191624432,1.3,-0.825000000000001));
#10060=CARTESIAN_POINT('Ctrl Pts',(-1.4132207435299,1.3,-0.852229869895949));
#10061=CARTESIAN_POINT('Ctrl Pts',(-1.39561049050871,1.30629366210296,-0.880751161609749));
#10062=CARTESIAN_POINT('Ctrl Pts',(-1.36172049302549,1.33182222741682,-0.932292094146256));
#10063=CARTESIAN_POINT('Ctrl Pts',(-1.34548213209931,1.35105447038507,-0.955340251466735));
#10064=CARTESIAN_POINT('Ctrl Pts',(-1.31917543061769,1.39539254159618,-0.991349264982991));
#10065=CARTESIAN_POINT('Ctrl Pts',(-1.30734972067592,1.42347183818157,-1.00672880483252));
#10066=CARTESIAN_POINT('Ctrl Pts',(-1.29146042158868,1.48505200040818,-1.02703269653942));
#10067=CARTESIAN_POINT('Ctrl Pts',(-1.28744468918255,1.51855708359447,-1.03198167246111));
#10068=CARTESIAN_POINT('Ctrl Pts',(-1.28744468918255,1.55,-1.03198167246111));
#10069=CARTESIAN_POINT('',(-1.42894191624432,1.8,-0.825000000000001));
#10070=CARTESIAN_POINT('Ctrl Pts',(-1.42894191624432,1.8,-0.825000000000001));
#10071=CARTESIAN_POINT('Ctrl Pts',(-1.44466308895875,1.8,-0.797770130104052));
#10072=CARTESIAN_POINT('Ctrl Pts',(-1.46055812562105,1.79370633789704,-0.768258557763732));
#10073=CARTESIAN_POINT('Ctrl Pts',(-1.48824888379079,1.76817777258318,-0.713138492740816));
#10074=CARTESIAN_POINT('Ctrl Pts',(-1.50008999307766,1.74894552961493,-0.687551581002689));
#10075=CARTESIAN_POINT('Ctrl Pts',(-1.51812136280714,1.70460745840382,-0.646764802471699));
#10076=CARTESIAN_POINT('Ctrl Pts',(-1.52552758004446,1.67652816181843,-0.628833667319578));
#10077=CARTESIAN_POINT('Ctrl Pts',(-1.53516661651472,1.61494799959182,-0.60492118480825));
#10078=CARTESIAN_POINT('Ctrl Pts',(-1.53744468918255,1.58144291640553,-0.598968970568896));
#10079=CARTESIAN_POINT('Ctrl Pts',(-1.53744468918255,1.51855708359447,-0.598968970568896));
#10080=CARTESIAN_POINT('Ctrl Pts',(-1.53516661651472,1.48505200040818,-0.60492118480825));
#10081=CARTESIAN_POINT('Ctrl Pts',(-1.52552758004446,1.42347183818157,-0.628833667319578));
#10082=CARTESIAN_POINT('Ctrl Pts',(-1.51812136280714,1.39539254159618,-0.646764802471699));
#10083=CARTESIAN_POINT('Ctrl Pts',(-1.50008999307766,1.35105447038507,-0.687551581002689));
#10084=CARTESIAN_POINT('Ctrl Pts',(-1.48824888379079,1.33182222741682,-0.713138492740816));
#10085=CARTESIAN_POINT('Ctrl Pts',(-1.46055812562105,1.30629366210296,-0.768258557763732));
#10086=CARTESIAN_POINT('Ctrl Pts',(-1.44466308895875,1.3,-0.797770130104052));
#10087=CARTESIAN_POINT('Ctrl Pts',(-1.42894191624432,1.3,-0.825000000000001));
#10088=CARTESIAN_POINT('Ctrl Pts',(-1.28744468918255,1.55,-1.03198167246111));
#10089=CARTESIAN_POINT('Ctrl Pts',(-1.28744468918255,1.58144291640553,-1.03198167246111));
#10090=CARTESIAN_POINT('Ctrl Pts',(-1.29146042158868,1.61494799959182,-1.02703269653942));
#10091=CARTESIAN_POINT('Ctrl Pts',(-1.30734972067592,1.67652816181843,-1.00672880483252));
#10092=CARTESIAN_POINT('Ctrl Pts',(-1.31917543061769,1.70460745840382,-0.991349264982991));
#10093=CARTESIAN_POINT('Ctrl Pts',(-1.34548213209931,1.74894552961493,-0.955340251466734));
#10094=CARTESIAN_POINT('Ctrl Pts',(-1.36172049302549,1.76817777258318,-0.932292094146256));
#10095=CARTESIAN_POINT('Ctrl Pts',(-1.39561049050871,1.79370633789704,-0.880751161609749));
#10096=CARTESIAN_POINT('Ctrl Pts',(-1.4132207435299,1.8,-0.852229869895949));
#10097=CARTESIAN_POINT('Ctrl Pts',(-1.42894191624432,1.8,-0.825000000000001));
#10098=CARTESIAN_POINT('Origin',(0.,1.55,0.));
#10099=CARTESIAN_POINT('',(-1.65,0.85,-2.02066721859313E-16));
#10100=CARTESIAN_POINT('Origin',(0.,0.85,0.));
#10101=CARTESIAN_POINT('',(-1.65,2.25,-2.02066721859313E-16));
#10102=CARTESIAN_POINT('',(-1.65,1.55,-2.02066721859313E-16));
#10103=CARTESIAN_POINT('Origin',(0.,2.25,0.));
#10104=CARTESIAN_POINT('',(-1.42894191624432,1.3,0.825));
#10105=CARTESIAN_POINT('',(-1.42894191624432,1.8,0.825));
#10106=CARTESIAN_POINT('Ctrl Pts',(-1.42894191624432,1.3,0.825));
#10107=CARTESIAN_POINT('Ctrl Pts',(-1.44466308895875,1.3,0.797770130104051));
#10108=CARTESIAN_POINT('Ctrl Pts',(-1.46055812562105,1.30629366210296,0.768258557763731));
#10109=CARTESIAN_POINT('Ctrl Pts',(-1.48824888379079,1.33182222741682,0.713138492740815));
#10110=CARTESIAN_POINT('Ctrl Pts',(-1.50008999307766,1.35105447038507,0.687551581002688));
#10111=CARTESIAN_POINT('Ctrl Pts',(-1.51812136280714,1.39539254159618,0.646764802471698));
#10112=CARTESIAN_POINT('Ctrl Pts',(-1.52552758004446,1.42347183818157,0.628833667319577));
#10113=CARTESIAN_POINT('Ctrl Pts',(-1.53516661651472,1.48505200040818,0.604921184808249));
#10114=CARTESIAN_POINT('Ctrl Pts',(-1.53744468918255,1.51855708359447,0.598968970568895));
#10115=CARTESIAN_POINT('Ctrl Pts',(-1.53744468918255,1.58144291640553,0.598968970568895));
#10116=CARTESIAN_POINT('Ctrl Pts',(-1.53516661651472,1.61494799959182,0.604921184808249));
#10117=CARTESIAN_POINT('Ctrl Pts',(-1.52552758004446,1.67652816181843,0.628833667319577));
#10118=CARTESIAN_POINT('Ctrl Pts',(-1.51812136280714,1.70460745840382,0.646764802471698));
#10119=CARTESIAN_POINT('Ctrl Pts',(-1.50008999307766,1.74894552961493,0.687551581002688));
#10120=CARTESIAN_POINT('Ctrl Pts',(-1.48824888379079,1.76817777258318,0.713138492740815));
#10121=CARTESIAN_POINT('Ctrl Pts',(-1.46055812562105,1.79370633789704,0.768258557763731));
#10122=CARTESIAN_POINT('Ctrl Pts',(-1.44466308895875,1.8,0.797770130104051));
#10123=CARTESIAN_POINT('Ctrl Pts',(-1.42894191624432,1.8,0.825));
#10124=CARTESIAN_POINT('',(-1.28744468918255,1.55,1.03198167246111));
#10125=CARTESIAN_POINT('Ctrl Pts',(-1.42894191624432,1.8,0.825));
#10126=CARTESIAN_POINT('Ctrl Pts',(-1.4132207435299,1.8,0.852229869895948));
#10127=CARTESIAN_POINT('Ctrl Pts',(-1.39561049050871,1.79370633789704,0.880751161609747));
#10128=CARTESIAN_POINT('Ctrl Pts',(-1.36172049302549,1.76817777258318,0.932292094146255));
#10129=CARTESIAN_POINT('Ctrl Pts',(-1.34548213209931,1.74894552961493,0.955340251466733));
#10130=CARTESIAN_POINT('Ctrl Pts',(-1.31917543061769,1.70460745840382,0.991349264982989));
#10131=CARTESIAN_POINT('Ctrl Pts',(-1.30734972067592,1.67652816181843,1.00672880483252));
#10132=CARTESIAN_POINT('Ctrl Pts',(-1.29146042158868,1.61494799959182,1.02703269653942));
#10133=CARTESIAN_POINT('Ctrl Pts',(-1.28744468918255,1.58144291640553,1.03198167246111));
#10134=CARTESIAN_POINT('Ctrl Pts',(-1.28744468918255,1.55,1.03198167246111));
#10135=CARTESIAN_POINT('Ctrl Pts',(-1.28744468918255,1.55,1.03198167246111));
#10136=CARTESIAN_POINT('Ctrl Pts',(-1.28744468918255,1.51855708359447,1.03198167246111));
#10137=CARTESIAN_POINT('Ctrl Pts',(-1.29146042158868,1.48505200040818,1.02703269653942));
#10138=CARTESIAN_POINT('Ctrl Pts',(-1.30734972067592,1.42347183818157,1.00672880483252));
#10139=CARTESIAN_POINT('Ctrl Pts',(-1.31917543061769,1.39539254159618,0.99134926498299));
#10140=CARTESIAN_POINT('Ctrl Pts',(-1.34548213209931,1.35105447038508,0.955340251466733));
#10141=CARTESIAN_POINT('Ctrl Pts',(-1.36172049302549,1.33182222741682,0.932292094146255));
#10142=CARTESIAN_POINT('Ctrl Pts',(-1.39561049050871,1.30629366210296,0.880751161609748));
#10143=CARTESIAN_POINT('Ctrl Pts',(-1.4132207435299,1.3,0.852229869895949));
#10144=CARTESIAN_POINT('Ctrl Pts',(-1.42894191624432,1.3,0.825));
#10145=CARTESIAN_POINT('',(1.42894191624432,1.8,-0.825));
#10146=CARTESIAN_POINT('',(1.42894191624432,1.3,-0.825));
#10147=CARTESIAN_POINT('Ctrl Pts',(1.42894191624432,1.8,-0.825));
#10148=CARTESIAN_POINT('Ctrl Pts',(1.4132207435299,1.8,-0.852229869895949));
#10149=CARTESIAN_POINT('Ctrl Pts',(1.39561049050871,1.79370633789704,-0.880751161609748));
#10150=CARTESIAN_POINT('Ctrl Pts',(1.36172049302549,1.76817777258318,-0.932292094146255));
#10151=CARTESIAN_POINT('Ctrl Pts',(1.34548213209931,1.74894552961493,-0.955340251466734));
#10152=CARTESIAN_POINT('Ctrl Pts',(1.31917543061769,1.70460745840382,-0.99134926498299));
#10153=CARTESIAN_POINT('Ctrl Pts',(1.30734972067592,1.67652816181843,-1.00672880483252));
#10154=CARTESIAN_POINT('Ctrl Pts',(1.29146042158868,1.61494799959182,-1.02703269653942));
#10155=CARTESIAN_POINT('Ctrl Pts',(1.28744468918255,1.58144291640553,-1.03198167246111));
#10156=CARTESIAN_POINT('Ctrl Pts',(1.28744468918255,1.51855708359447,-1.03198167246111));
#10157=CARTESIAN_POINT('Ctrl Pts',(1.29146042158868,1.48505200040818,-1.02703269653942));
#10158=CARTESIAN_POINT('Ctrl Pts',(1.30734972067592,1.42347183818157,-1.00672880483252));
#10159=CARTESIAN_POINT('Ctrl Pts',(1.31917543061769,1.39539254159618,-0.99134926498299));
#10160=CARTESIAN_POINT('Ctrl Pts',(1.34548213209931,1.35105447038507,-0.955340251466734));
#10161=CARTESIAN_POINT('Ctrl Pts',(1.36172049302549,1.33182222741682,-0.932292094146255));
#10162=CARTESIAN_POINT('Ctrl Pts',(1.39561049050871,1.30629366210296,-0.880751161609748));
#10163=CARTESIAN_POINT('Ctrl Pts',(1.4132207435299,1.3,-0.852229869895948));
#10164=CARTESIAN_POINT('Ctrl Pts',(1.42894191624432,1.3,-0.825));
#10165=CARTESIAN_POINT('',(1.53744468918255,1.55,-0.598968970568895));
#10166=CARTESIAN_POINT('Ctrl Pts',(1.42894191624432,1.3,-0.825));
#10167=CARTESIAN_POINT('Ctrl Pts',(1.44466308895875,1.3,-0.797770130104051));
#10168=CARTESIAN_POINT('Ctrl Pts',(1.46055812562105,1.30629366210296,-0.768258557763731));
#10169=CARTESIAN_POINT('Ctrl Pts',(1.48824888379079,1.33182222741682,-0.713138492740815));
#10170=CARTESIAN_POINT('Ctrl Pts',(1.50008999307766,1.35105447038507,-0.687551581002688));
#10171=CARTESIAN_POINT('Ctrl Pts',(1.51812136280714,1.39539254159618,-0.646764802471698));
#10172=CARTESIAN_POINT('Ctrl Pts',(1.52552758004446,1.42347183818157,-0.628833667319577));
#10173=CARTESIAN_POINT('Ctrl Pts',(1.53516661651472,1.48505200040818,-0.604921184808249));
#10174=CARTESIAN_POINT('Ctrl Pts',(1.53744468918255,1.51855708359447,-0.598968970568895));
#10175=CARTESIAN_POINT('Ctrl Pts',(1.53744468918255,1.55,-0.598968970568895));
#10176=CARTESIAN_POINT('Ctrl Pts',(1.53744468918255,1.55,-0.598968970568895));
#10177=CARTESIAN_POINT('Ctrl Pts',(1.53744468918255,1.58144291640553,-0.598968970568895));
#10178=CARTESIAN_POINT('Ctrl Pts',(1.53516661651472,1.61494799959182,-0.604921184808249));
#10179=CARTESIAN_POINT('Ctrl Pts',(1.52552758004446,1.67652816181843,-0.628833667319577));
#10180=CARTESIAN_POINT('Ctrl Pts',(1.51812136280714,1.70460745840382,-0.646764802471698));
#10181=CARTESIAN_POINT('Ctrl Pts',(1.50008999307766,1.74894552961493,-0.687551581002688));
#10182=CARTESIAN_POINT('Ctrl Pts',(1.48824888379079,1.76817777258318,-0.713138492740815));
#10183=CARTESIAN_POINT('Ctrl Pts',(1.46055812562105,1.79370633789704,-0.768258557763731));
#10184=CARTESIAN_POINT('Ctrl Pts',(1.44466308895875,1.8,-0.797770130104051));
#10185=CARTESIAN_POINT('Ctrl Pts',(1.42894191624432,1.8,-0.825));
#10186=CARTESIAN_POINT('',(0.,1.3,-1.65));
#10187=CARTESIAN_POINT('',(0.,1.8,-1.65));
#10188=CARTESIAN_POINT('Ctrl Pts',(1.38777878078145E-17,1.3,-1.65));
#10189=CARTESIAN_POINT('Ctrl Pts',(0.0314423454288489,1.3,-1.65));
#10190=CARTESIAN_POINT('Ctrl Pts',(0.0649476351123396,1.30629366210296,
-1.64900971937348));
#10191=CARTESIAN_POINT('Ctrl Pts',(0.126528390765307,1.33182222741682,-1.64543058688707));
#10192=CARTESIAN_POINT('Ctrl Pts',(0.154607860978348,1.35105447038507,-1.64289183246942));
#10193=CARTESIAN_POINT('Ctrl Pts',(0.198945932189457,1.39539254159618,-1.63811406745469));
#10194=CARTESIAN_POINT('Ctrl Pts',(0.218177859368546,1.42347183818157,-1.63556247215209));
#10195=CARTESIAN_POINT('Ctrl Pts',(0.243706194926033,1.48505200040818,-1.63195388134767));
#10196=CARTESIAN_POINT('Ctrl Pts',(0.25,1.51855708359447,-1.63095064303001));
#10197=CARTESIAN_POINT('Ctrl Pts',(0.25,1.58144291640553,-1.63095064303001));
#10198=CARTESIAN_POINT('Ctrl Pts',(0.243706194926033,1.61494799959182,-1.63195388134767));
#10199=CARTESIAN_POINT('Ctrl Pts',(0.218177859368546,1.67652816181843,-1.63556247215209));
#10200=CARTESIAN_POINT('Ctrl Pts',(0.198945932189457,1.70460745840382,-1.63811406745469));
#10201=CARTESIAN_POINT('Ctrl Pts',(0.154607860978349,1.74894552961493,-1.64289183246942));
#10202=CARTESIAN_POINT('Ctrl Pts',(0.126528390765307,1.76817777258318,-1.64543058688707));
#10203=CARTESIAN_POINT('Ctrl Pts',(0.0649476351123398,1.79370633789704,
-1.64900971937348));
#10204=CARTESIAN_POINT('Ctrl Pts',(0.031442345428849,1.8,-1.65));
#10205=CARTESIAN_POINT('Ctrl Pts',(7.63278329429795E-17,1.8,-1.65));
#10206=CARTESIAN_POINT('',(-0.25,1.55,-1.63095064303001));
#10207=CARTESIAN_POINT('Ctrl Pts',(9.0205620750794E-17,1.8,-1.65));
#10208=CARTESIAN_POINT('Ctrl Pts',(-0.0314423454288488,1.8,-1.65));
#10209=CARTESIAN_POINT('Ctrl Pts',(-0.0649476351123396,1.79370633789704,
-1.64900971937348));
#10210=CARTESIAN_POINT('Ctrl Pts',(-0.126528390765307,1.76817777258318,
-1.64543058688707));
#10211=CARTESIAN_POINT('Ctrl Pts',(-0.154607860978348,1.74894552961493,
-1.64289183246942));
#10212=CARTESIAN_POINT('Ctrl Pts',(-0.198945932189456,1.70460745840382,
-1.63811406745469));
#10213=CARTESIAN_POINT('Ctrl Pts',(-0.218177859368546,1.67652816181843,
-1.63556247215209));
#10214=CARTESIAN_POINT('Ctrl Pts',(-0.243706194926033,1.61494799959182,
-1.63195388134767));
#10215=CARTESIAN_POINT('Ctrl Pts',(-0.25,1.58144291640553,-1.63095064303001));
#10216=CARTESIAN_POINT('Ctrl Pts',(-0.25,1.55,-1.63095064303001));
#10217=CARTESIAN_POINT('Ctrl Pts',(-0.25,1.55,-1.63095064303001));
#10218=CARTESIAN_POINT('Ctrl Pts',(-0.25,1.51855708359447,-1.63095064303001));
#10219=CARTESIAN_POINT('Ctrl Pts',(-0.243706194926033,1.48505200040818,
-1.63195388134767));
#10220=CARTESIAN_POINT('Ctrl Pts',(-0.218177859368546,1.42347183818157,
-1.63556247215209));
#10221=CARTESIAN_POINT('Ctrl Pts',(-0.198945932189457,1.39539254159618,
-1.63811406745469));
#10222=CARTESIAN_POINT('Ctrl Pts',(-0.154607860978349,1.35105447038507,
-1.64289183246942));
#10223=CARTESIAN_POINT('Ctrl Pts',(-0.126528390765307,1.33182222741682,
-1.64543058688707));
#10224=CARTESIAN_POINT('Ctrl Pts',(-0.0649476351123398,1.30629366210296,
-1.64900971937348));
#10225=CARTESIAN_POINT('Ctrl Pts',(-0.031442345428849,1.3,-1.65));
#10226=CARTESIAN_POINT('Ctrl Pts',(-4.85722573273506E-17,1.3,-1.65));
#10227=CARTESIAN_POINT('',(0.,1.8,1.65));
#10228=CARTESIAN_POINT('',(0.,1.3,1.65));
#10229=CARTESIAN_POINT('Ctrl Pts',(8.32667268468867E-17,1.8,1.65));
#10230=CARTESIAN_POINT('Ctrl Pts',(0.031442345428849,1.8,1.65));
#10231=CARTESIAN_POINT('Ctrl Pts',(0.0649476351123398,1.79370633789704,
1.64900971937348));
#10232=CARTESIAN_POINT('Ctrl Pts',(0.126528390765307,1.76817777258318,1.64543058688707));
#10233=CARTESIAN_POINT('Ctrl Pts',(0.154607860978349,1.74894552961493,1.64289183246942));
#10234=CARTESIAN_POINT('Ctrl Pts',(0.198945932189457,1.70460745840382,1.63811406745469));
#10235=CARTESIAN_POINT('Ctrl Pts',(0.218177859368546,1.67652816181843,1.63556247215209));
#10236=CARTESIAN_POINT('Ctrl Pts',(0.243706194926033,1.61494799959182,1.63195388134767));
#10237=CARTESIAN_POINT('Ctrl Pts',(0.25,1.58144291640553,1.63095064303001));
#10238=CARTESIAN_POINT('Ctrl Pts',(0.25,1.51855708359447,1.63095064303001));
#10239=CARTESIAN_POINT('Ctrl Pts',(0.243706194926033,1.48505200040818,1.63195388134767));
#10240=CARTESIAN_POINT('Ctrl Pts',(0.218177859368546,1.42347183818157,1.63556247215209));
#10241=CARTESIAN_POINT('Ctrl Pts',(0.198945932189457,1.39539254159618,1.63811406745469));
#10242=CARTESIAN_POINT('Ctrl Pts',(0.154607860978348,1.35105447038507,1.64289183246942));
#10243=CARTESIAN_POINT('Ctrl Pts',(0.126528390765307,1.33182222741682,1.64543058688707));
#10244=CARTESIAN_POINT('Ctrl Pts',(0.0649476351123397,1.30629366210296,
1.64900971937348));
#10245=CARTESIAN_POINT('Ctrl Pts',(0.0314423454288488,1.3,1.65));
#10246=CARTESIAN_POINT('Ctrl Pts',(-1.38777878078145E-17,1.3,1.65));
#10247=CARTESIAN_POINT('',(-0.25,1.55,1.63095064303001));
#10248=CARTESIAN_POINT('Ctrl Pts',(-5.55111512312578E-17,1.3,1.65));
#10249=CARTESIAN_POINT('Ctrl Pts',(-0.031442345428849,1.3,1.65));
#10250=CARTESIAN_POINT('Ctrl Pts',(-0.0649476351123398,1.30629366210296,
1.64900971937348));
#10251=CARTESIAN_POINT('Ctrl Pts',(-0.126528390765307,1.33182222741682,
1.64543058688707));
#10252=CARTESIAN_POINT('Ctrl Pts',(-0.154607860978349,1.35105447038507,
1.64289183246942));
#10253=CARTESIAN_POINT('Ctrl Pts',(-0.198945932189457,1.39539254159618,
1.63811406745469));
#10254=CARTESIAN_POINT('Ctrl Pts',(-0.218177859368546,1.42347183818157,
1.63556247215209));
#10255=CARTESIAN_POINT('Ctrl Pts',(-0.243706194926033,1.48505200040818,
1.63195388134767));
#10256=CARTESIAN_POINT('Ctrl Pts',(-0.25,1.51855708359447,1.63095064303001));
#10257=CARTESIAN_POINT('Ctrl Pts',(-0.25,1.55,1.63095064303001));
#10258=CARTESIAN_POINT('Ctrl Pts',(-0.25,1.55,1.63095064303001));
#10259=CARTESIAN_POINT('Ctrl Pts',(-0.25,1.58144291640553,1.63095064303001));
#10260=CARTESIAN_POINT('Ctrl Pts',(-0.243706194926033,1.61494799959182,
1.63195388134767));
#10261=CARTESIAN_POINT('Ctrl Pts',(-0.218177859368546,1.67652816181843,
1.63556247215209));
#10262=CARTESIAN_POINT('Ctrl Pts',(-0.198945932189456,1.70460745840382,
1.63811406745469));
#10263=CARTESIAN_POINT('Ctrl Pts',(-0.154607860978348,1.74894552961493,
1.64289183246942));
#10264=CARTESIAN_POINT('Ctrl Pts',(-0.126528390765307,1.76817777258318,
1.64543058688707));
#10265=CARTESIAN_POINT('Ctrl Pts',(-0.0649476351123396,1.79370633789704,
1.64900971937348));
#10266=CARTESIAN_POINT('Ctrl Pts',(-0.0314423454288488,1.8,1.65));
#10267=CARTESIAN_POINT('Ctrl Pts',(7.63278329429795E-17,1.8,1.65));
#10268=CARTESIAN_POINT('Origin',(0.,1.55,0.));
#10269=CARTESIAN_POINT('',(-0.713525491562421,1.55,0.700629269222037));
#10270=CARTESIAN_POINT('',(0.125,1.55,0.21650635094611));
#10271=CARTESIAN_POINT('Ctrl Pts',(-0.713525491562421,1.55,0.700629269222037));
#10272=CARTESIAN_POINT('Ctrl Pts',(-0.713525491562421,1.5815373526696,0.700629269222037));
#10273=CARTESIAN_POINT('Ctrl Pts',(-0.718163997970498,1.61508042700263,
0.695997784676727));
#10274=CARTESIAN_POINT('Ctrl Pts',(-0.73619249062986,1.67663267125761,0.676899590973058));
#10275=CARTESIAN_POINT('Ctrl Pts',(-0.749495710301795,1.70465411363682,
0.662390652284073));
#10276=CARTESIAN_POINT('Ctrl Pts',(-0.778498278845144,1.74889618382539,
0.628048950774009));
#10277=CARTESIAN_POINT('Ctrl Pts',(-0.796153444118959,1.76811531482682,
0.605884303066698));
#10278=CARTESIAN_POINT('Ctrl Pts',(-0.832065554235658,1.79367084275751,
0.555538485325663));
#10279=CARTESIAN_POINT('Ctrl Pts',(-0.850258932191534,1.8,0.527308329855002));
#10280=CARTESIAN_POINT('Ctrl Pts',(-0.881791875377343,1.8,0.472691670144998));
#10281=CARTESIAN_POINT('Ctrl Pts',(-0.897143218189782,1.79367084275751,
0.442820664919227));
#10282=CARTESIAN_POINT('Ctrl Pts',(-0.92278792026947,1.76811531482682,0.386546956384144));
#10283=CARTESIAN_POINT('Ctrl Pts',(-0.933155485613026,1.74889618382539,
0.360174810895352));
#10284=CARTESIAN_POINT('Ctrl Pts',(-0.948394987258249,1.70465411363682,
0.31788699900678));
#10285=CARTESIAN_POINT('Ctrl Pts',(-0.954308486908894,1.67663267125761,
0.299111603474267));
#10286=CARTESIAN_POINT('Ctrl Pts',(-0.961833761492987,1.61508042700263,
0.273949373987484));
#10287=CARTESIAN_POINT('Ctrl Pts',(-0.963525491562421,1.5815373526696,0.267616567329817));
#10288=CARTESIAN_POINT('Ctrl Pts',(-0.963525491562421,1.5184626473304,0.267616567329817));
#10289=CARTESIAN_POINT('Ctrl Pts',(-0.961833761492987,1.48491957299737,
0.273949373987484));
#10290=CARTESIAN_POINT('Ctrl Pts',(-0.954308486908894,1.42336732874239,
0.299111603474267));
#10291=CARTESIAN_POINT('Ctrl Pts',(-0.948394987258249,1.39534588636318,
0.31788699900678));
#10292=CARTESIAN_POINT('Ctrl Pts',(-0.933155485613026,1.35110381617461,
0.360174810895352));
#10293=CARTESIAN_POINT('Ctrl Pts',(-0.92278792026947,1.33188468517318,0.386546956384144));
#10294=CARTESIAN_POINT('Ctrl Pts',(-0.897143218189782,1.30632915724249,
0.442820664919227));
#10295=CARTESIAN_POINT('Ctrl Pts',(-0.881791875377343,1.3,0.472691670144998));
#10296=CARTESIAN_POINT('Ctrl Pts',(-0.850258932191534,1.3,0.527308329855002));
#10297=CARTESIAN_POINT('Ctrl Pts',(-0.832065554235658,1.30632915724249,
0.555538485325663));
#10298=CARTESIAN_POINT('Ctrl Pts',(-0.796153444118959,1.33188468517318,
0.605884303066698));
#10299=CARTESIAN_POINT('Ctrl Pts',(-0.778498278845144,1.35110381617461,
0.628048950774009));
#10300=CARTESIAN_POINT('Ctrl Pts',(-0.749495710301795,1.39534588636318,
0.662390652284073));
#10301=CARTESIAN_POINT('Ctrl Pts',(-0.73619249062986,1.42336732874239,0.676899590973058));
#10302=CARTESIAN_POINT('Ctrl Pts',(-0.718163997970498,1.48491957299737,
0.695997784676727));
#10303=CARTESIAN_POINT('Ctrl Pts',(-0.713525491562421,1.5184626473304,0.700629269222037));
#10304=CARTESIAN_POINT('Ctrl Pts',(-0.713525491562421,1.55,0.700629269222037));
#10305=CARTESIAN_POINT('Origin',(0.,1.55,0.));
#10306=CARTESIAN_POINT('',(0.963525491562421,1.55,-0.267616567329817));
#10307=CARTESIAN_POINT('Ctrl Pts',(0.963525491562421,1.55,-0.267616567329817));
#10308=CARTESIAN_POINT('Ctrl Pts',(0.963525491562421,1.5184626473304,-0.267616567329817));
#10309=CARTESIAN_POINT('Ctrl Pts',(0.961833761492987,1.48491957299737,-0.273949373987484));
#10310=CARTESIAN_POINT('Ctrl Pts',(0.954308486908894,1.42336732874239,-0.299111603474267));
#10311=CARTESIAN_POINT('Ctrl Pts',(0.948394987258249,1.39534588636318,-0.31788699900678));
#10312=CARTESIAN_POINT('Ctrl Pts',(0.933155485613026,1.35110381617461,-0.360174810895352));
#10313=CARTESIAN_POINT('Ctrl Pts',(0.92278792026947,1.33188468517318,-0.386546956384144));
#10314=CARTESIAN_POINT('Ctrl Pts',(0.897143218189782,1.30632915724249,-0.442820664919227));
#10315=CARTESIAN_POINT('Ctrl Pts',(0.881791875377343,1.3,-0.472691670144998));
#10316=CARTESIAN_POINT('Ctrl Pts',(0.850258932191534,1.3,-0.527308329855002));
#10317=CARTESIAN_POINT('Ctrl Pts',(0.832065554235658,1.30632915724249,-0.555538485325663));
#10318=CARTESIAN_POINT('Ctrl Pts',(0.796153444118959,1.33188468517318,-0.605884303066698));
#10319=CARTESIAN_POINT('Ctrl Pts',(0.778498278845144,1.35110381617461,-0.628048950774009));
#10320=CARTESIAN_POINT('Ctrl Pts',(0.749495710301795,1.39534588636318,-0.662390652284073));
#10321=CARTESIAN_POINT('Ctrl Pts',(0.73619249062986,1.42336732874239,-0.676899590973058));
#10322=CARTESIAN_POINT('Ctrl Pts',(0.718163997970498,1.48491957299737,-0.695997784676727));
#10323=CARTESIAN_POINT('Ctrl Pts',(0.713525491562421,1.5184626473304,-0.700629269222037));
#10324=CARTESIAN_POINT('Ctrl Pts',(0.713525491562421,1.5815373526696,-0.700629269222037));
#10325=CARTESIAN_POINT('Ctrl Pts',(0.718163997970498,1.61508042700263,-0.695997784676727));
#10326=CARTESIAN_POINT('Ctrl Pts',(0.73619249062986,1.67663267125761,-0.676899590973058));
#10327=CARTESIAN_POINT('Ctrl Pts',(0.749495710301795,1.70465411363682,-0.662390652284073));
#10328=CARTESIAN_POINT('Ctrl Pts',(0.778498278845144,1.74889618382539,-0.628048950774009));
#10329=CARTESIAN_POINT('Ctrl Pts',(0.796153444118959,1.76811531482682,-0.605884303066698));
#10330=CARTESIAN_POINT('Ctrl Pts',(0.832065554235658,1.79367084275751,-0.555538485325663));
#10331=CARTESIAN_POINT('Ctrl Pts',(0.850258932191534,1.8,-0.527308329855002));
#10332=CARTESIAN_POINT('Ctrl Pts',(0.881791875377343,1.8,-0.472691670144998));
#10333=CARTESIAN_POINT('Ctrl Pts',(0.897143218189782,1.79367084275751,-0.442820664919227));
#10334=CARTESIAN_POINT('Ctrl Pts',(0.92278792026947,1.76811531482682,-0.386546956384144));
#10335=CARTESIAN_POINT('Ctrl Pts',(0.933155485613026,1.74889618382539,-0.360174810895352));
#10336=CARTESIAN_POINT('Ctrl Pts',(0.948394987258249,1.70465411363682,-0.31788699900678));
#10337=CARTESIAN_POINT('Ctrl Pts',(0.954308486908894,1.67663267125761,-0.299111603474267));
#10338=CARTESIAN_POINT('Ctrl Pts',(0.961833761492987,1.61508042700263,-0.273949373987484));
#10339=CARTESIAN_POINT('Ctrl Pts',(0.963525491562421,1.5815373526696,-0.267616567329817));
#10340=CARTESIAN_POINT('Ctrl Pts',(0.963525491562421,1.55,-0.267616567329817));
#10341=CARTESIAN_POINT('',(0.125,1.55,0.21650635094611));
#10342=CARTESIAN_POINT('Origin',(0.,1.55,0.));
#10343=CARTESIAN_POINT('',(-0.25,1.55,-0.968245836551854));
#10344=CARTESIAN_POINT('',(-0.25,1.55,0.));
#10345=CARTESIAN_POINT('Ctrl Pts',(-0.25,1.55,-0.968245836551854));
#10346=CARTESIAN_POINT('Ctrl Pts',(-0.25,1.5815373526696,-0.968245836551854));
#10347=CARTESIAN_POINT('Ctrl Pts',(-0.243669763522489,1.61508042700263,
-0.969947158664211));
#10348=CARTESIAN_POINT('Ctrl Pts',(-0.218115996279034,1.67663267125761,
-0.976011194447325));
#10349=CARTESIAN_POINT('Ctrl Pts',(-0.198899276956455,1.70465411363682,
-0.980277651290853));
#10350=CARTESIAN_POINT('Ctrl Pts',(-0.154657206767882,1.74889618382539,
-0.988223761669361));
#10351=CARTESIAN_POINT('Ctrl Pts',(-0.126634476150511,1.76811531482682,
-0.992431259450842));
#10352=CARTESIAN_POINT('Ctrl Pts',(-0.0650776639541238,1.79367084275751,
-0.99835915024489));
#10353=CARTESIAN_POINT('Ctrl Pts',(-0.0315329431858092,1.8,-1.));
#10354=CARTESIAN_POINT('Ctrl Pts',(0.0315329431858092,1.8,-1.));
#10355=CARTESIAN_POINT('Ctrl Pts',(0.0650776639541238,1.79367084275751,
-0.99835915024489));
#10356=CARTESIAN_POINT('Ctrl Pts',(0.126634476150511,1.76811531482682,-0.992431259450842));
#10357=CARTESIAN_POINT('Ctrl Pts',(0.154657206767882,1.74889618382539,-0.988223761669361));
#10358=CARTESIAN_POINT('Ctrl Pts',(0.198899276956455,1.70465411363682,-0.980277651290853));
#10359=CARTESIAN_POINT('Ctrl Pts',(0.218115996279034,1.67663267125761,-0.976011194447325));
#10360=CARTESIAN_POINT('Ctrl Pts',(0.243669763522488,1.61508042700263,-0.969947158664211));
#10361=CARTESIAN_POINT('Ctrl Pts',(0.25,1.5815373526696,-0.968245836551854));
#10362=CARTESIAN_POINT('Ctrl Pts',(0.25,1.5184626473304,-0.968245836551854));
#10363=CARTESIAN_POINT('Ctrl Pts',(0.243669763522488,1.48491957299737,-0.969947158664211));
#10364=CARTESIAN_POINT('Ctrl Pts',(0.218115996279034,1.42336732874239,-0.976011194447325));
#10365=CARTESIAN_POINT('Ctrl Pts',(0.198899276956455,1.39534588636318,-0.980277651290853));
#10366=CARTESIAN_POINT('Ctrl Pts',(0.154657206767882,1.35110381617461,-0.988223761669361));
#10367=CARTESIAN_POINT('Ctrl Pts',(0.126634476150511,1.33188468517318,-0.992431259450842));
#10368=CARTESIAN_POINT('Ctrl Pts',(0.0650776639541239,1.30632915724249,
-0.99835915024489));
#10369=CARTESIAN_POINT('Ctrl Pts',(0.0315329431858092,1.3,-1.));
#10370=CARTESIAN_POINT('Ctrl Pts',(-0.0315329431858092,1.3,-1.));
#10371=CARTESIAN_POINT('Ctrl Pts',(-0.0650776639541239,1.30632915724249,
-0.99835915024489));
#10372=CARTESIAN_POINT('Ctrl Pts',(-0.126634476150511,1.33188468517318,
-0.992431259450842));
#10373=CARTESIAN_POINT('Ctrl Pts',(-0.154657206767882,1.35110381617461,
-0.988223761669361));
#10374=CARTESIAN_POINT('Ctrl Pts',(-0.198899276956455,1.39534588636318,
-0.980277651290853));
#10375=CARTESIAN_POINT('Ctrl Pts',(-0.218115996279034,1.42336732874239,
-0.976011194447325));
#10376=CARTESIAN_POINT('Ctrl Pts',(-0.243669763522489,1.48491957299737,
-0.969947158664211));
#10377=CARTESIAN_POINT('Ctrl Pts',(-0.25,1.5184626473304,-0.968245836551854));
#10378=CARTESIAN_POINT('Ctrl Pts',(-0.25,1.55,-0.968245836551854));
#10379=CARTESIAN_POINT('Origin',(0.,1.55,0.));
#10380=CARTESIAN_POINT('',(-0.25,1.55,0.968245836551854));
#10381=CARTESIAN_POINT('Ctrl Pts',(-0.25,1.55,0.968245836551854));
#10382=CARTESIAN_POINT('Ctrl Pts',(-0.25,1.5184626473304,0.968245836551854));
#10383=CARTESIAN_POINT('Ctrl Pts',(-0.243669763522489,1.48491957299737,
0.969947158664211));
#10384=CARTESIAN_POINT('Ctrl Pts',(-0.218115996279034,1.42336732874239,
0.976011194447325));
#10385=CARTESIAN_POINT('Ctrl Pts',(-0.198899276956455,1.39534588636318,
0.980277651290853));
#10386=CARTESIAN_POINT('Ctrl Pts',(-0.154657206767882,1.35110381617461,
0.988223761669361));
#10387=CARTESIAN_POINT('Ctrl Pts',(-0.126634476150511,1.33188468517318,
0.992431259450842));
#10388=CARTESIAN_POINT('Ctrl Pts',(-0.065077663954124,1.30632915724249,
0.99835915024489));
#10389=CARTESIAN_POINT('Ctrl Pts',(-0.0315329431858092,1.3,1.));
#10390=CARTESIAN_POINT('Ctrl Pts',(0.0315329431858092,1.3,1.));
#10391=CARTESIAN_POINT('Ctrl Pts',(0.065077663954124,1.30632915724249,0.99835915024489));
#10392=CARTESIAN_POINT('Ctrl Pts',(0.126634476150511,1.33188468517318,0.992431259450842));
#10393=CARTESIAN_POINT('Ctrl Pts',(0.154657206767882,1.35110381617461,0.988223761669361));
#10394=CARTESIAN_POINT('Ctrl Pts',(0.198899276956455,1.39534588636318,0.980277651290853));
#10395=CARTESIAN_POINT('Ctrl Pts',(0.218115996279034,1.42336732874239,0.976011194447325));
#10396=CARTESIAN_POINT('Ctrl Pts',(0.243669763522488,1.48491957299737,0.969947158664211));
#10397=CARTESIAN_POINT('Ctrl Pts',(0.25,1.5184626473304,0.968245836551854));
#10398=CARTESIAN_POINT('Ctrl Pts',(0.25,1.5815373526696,0.968245836551854));
#10399=CARTESIAN_POINT('Ctrl Pts',(0.243669763522488,1.61508042700263,0.969947158664211));
#10400=CARTESIAN_POINT('Ctrl Pts',(0.218115996279034,1.67663267125761,0.976011194447325));
#10401=CARTESIAN_POINT('Ctrl Pts',(0.198899276956455,1.70465411363682,0.980277651290853));
#10402=CARTESIAN_POINT('Ctrl Pts',(0.154657206767882,1.74889618382539,0.988223761669361));
#10403=CARTESIAN_POINT('Ctrl Pts',(0.126634476150511,1.76811531482682,0.992431259450842));
#10404=CARTESIAN_POINT('Ctrl Pts',(0.0650776639541239,1.79367084275751,
0.99835915024489));
#10405=CARTESIAN_POINT('Ctrl Pts',(0.0315329431858092,1.8,1.));
#10406=CARTESIAN_POINT('Ctrl Pts',(-0.0315329431858092,1.8,1.));
#10407=CARTESIAN_POINT('Ctrl Pts',(-0.0650776639541239,1.79367084275751,
0.99835915024489));
#10408=CARTESIAN_POINT('Ctrl Pts',(-0.126634476150511,1.76811531482682,
0.992431259450842));
#10409=CARTESIAN_POINT('Ctrl Pts',(-0.154657206767882,1.74889618382539,
0.988223761669361));
#10410=CARTESIAN_POINT('Ctrl Pts',(-0.198899276956455,1.70465411363682,
0.980277651290853));
#10411=CARTESIAN_POINT('Ctrl Pts',(-0.218115996279034,1.67663267125761,
0.976011194447325));
#10412=CARTESIAN_POINT('Ctrl Pts',(-0.243669763522489,1.61508042700263,
0.969947158664211));
#10413=CARTESIAN_POINT('Ctrl Pts',(-0.25,1.5815373526696,0.968245836551854));
#10414=CARTESIAN_POINT('Ctrl Pts',(-0.25,1.55,0.968245836551854));
#10415=CARTESIAN_POINT('',(-0.25,1.55,0.));
#10416=CARTESIAN_POINT('Origin',(1.65,2.25,0.));
#10417=CARTESIAN_POINT('',(-1.,2.25,-1.22464679914735E-16));
#10418=CARTESIAN_POINT('Origin',(0.,2.25,0.));
#10419=CARTESIAN_POINT('Origin',(1.75,0.85,0.));
#10420=CARTESIAN_POINT('',(-1.75,0.85,-2.14313189850787E-16));
#10421=CARTESIAN_POINT('Origin',(0.,0.85,0.));
#10422=CARTESIAN_POINT('Origin',(0.,0.,0.));
#10423=CARTESIAN_POINT('',(-1.75,-0.85,-2.14313189850787E-16));
#10424=CARTESIAN_POINT('Origin',(0.,-0.85,0.));
#10425=CARTESIAN_POINT('',(-1.75,0.,-2.14313189850787E-16));
#10426=CARTESIAN_POINT('Origin',(1.,-0.85,0.));
#10427=CARTESIAN_POINT('',(-1.,-0.85,-1.22464679914735E-16));
#10428=CARTESIAN_POINT('Origin',(0.,-0.85,0.));
#10429=CARTESIAN_POINT('Origin',(0.,0.7,0.));
#10430=CARTESIAN_POINT('',(-1.,0.7,-1.22464679914735E-16));
#10431=CARTESIAN_POINT('',(0.,0.,0.));
#10432=CARTESIAN_POINT('',(0.,0.,0.));
#10433=CARTESIAN_POINT('',(0.,0.,0.));
#10434=CARTESIAN_POINT('Origin',(0.,0.,0.));
#10435=CARTESIAN_POINT('',(-0.42,0.16,5.14351655641888E-17));
#10436=CARTESIAN_POINT('Origin',(0.,0.16,0.));
#10437=CARTESIAN_POINT('',(-0.42,0.,5.14351655641888E-17));
#10438=CARTESIAN_POINT('',(-0.42,0.,5.14351655641888E-17));
#10439=CARTESIAN_POINT('Origin',(0.,0.,0.));
#10440=CARTESIAN_POINT('Origin',(0.,0.,0.));
#10441=CARTESIAN_POINT('',(-0.8,0.16,9.79717439317883E-17));
#10442=CARTESIAN_POINT('Origin',(0.,0.16,0.));
#10443=CARTESIAN_POINT('',(-0.8,0.,9.79717439317883E-17));
#10444=CARTESIAN_POINT('',(-0.8,0.,9.79717439317883E-17));
#10445=CARTESIAN_POINT('Origin',(0.,0.,0.));
#10446=CARTESIAN_POINT('Origin',(0.,0.16,0.));
#10447=CARTESIAN_POINT('Origin',(0.,0.,0.));
#10448=CARTESIAN_POINT('',(0.,0.,0.));
#10449=CARTESIAN_POINT('Origin',(0.173205080756888,-0.8,-0.3));
#10450=CARTESIAN_POINT('',(0.346410161513775,-0.8,0.));
#10451=CARTESIAN_POINT('',(0.173205080756888,-0.8,-0.3));
#10452=CARTESIAN_POINT('',(0.346410161513775,-0.8,0.));
#10453=CARTESIAN_POINT('',(0.173205080756888,-1.28,-0.3));
#10454=CARTESIAN_POINT('',(0.173205080756888,-0.8,-0.3));
#10455=CARTESIAN_POINT('',(0.346410161513775,-1.28,0.));
#10456=CARTESIAN_POINT('',(0.346410161513775,-1.28,0.));
#10457=CARTESIAN_POINT('',(0.346410161513775,-0.8,0.));
#10458=CARTESIAN_POINT('Origin',(-0.173205080756888,-0.8,-0.3));
#10459=CARTESIAN_POINT('',(-0.173205080756888,-0.8,-0.3));
#10460=CARTESIAN_POINT('',(0.173205080756888,-0.8,-0.3));
#10461=CARTESIAN_POINT('',(-0.173205080756888,-1.28,-0.3));
#10462=CARTESIAN_POINT('',(-0.173205080756888,-0.8,-0.3));
#10463=CARTESIAN_POINT('',(0.173205080756888,-1.28,-0.3));
#10464=CARTESIAN_POINT('Origin',(-0.346410161513775,-0.8,-5.55111512312578E-17));
#10465=CARTESIAN_POINT('',(-0.346410161513775,-0.8,-4.24230095489963E-17));
#10466=CARTESIAN_POINT('',(-0.173205080756888,-0.8,-0.3));
#10467=CARTESIAN_POINT('',(-0.346410161513775,-1.28,-5.55111512312578E-17));
#10468=CARTESIAN_POINT('',(-0.346410161513775,-0.8,-4.24230095489963E-17));
#10469=CARTESIAN_POINT('',(-0.173205080756888,-1.28,-0.3));
#10470=CARTESIAN_POINT('Origin',(-0.173205080756888,-0.8,0.3));
#10471=CARTESIAN_POINT('',(-0.173205080756888,-0.8,0.3));
#10472=CARTESIAN_POINT('',(-0.346410161513775,-0.8,-4.24230095489963E-17));
#10473=CARTESIAN_POINT('',(-0.173205080756888,-1.28,0.3));
#10474=CARTESIAN_POINT('',(-0.173205080756888,-0.8,0.3));
#10475=CARTESIAN_POINT('',(-0.346410161513775,-1.28,-4.24230095489963E-17));
#10476=CARTESIAN_POINT('Origin',(0.173205080756888,-0.8,0.3));
#10477=CARTESIAN_POINT('',(0.173205080756888,-0.8,0.3));
#10478=CARTESIAN_POINT('',(-0.173205080756888,-0.8,0.3));
#10479=CARTESIAN_POINT('',(0.173205080756888,-1.28,0.3));
#10480=CARTESIAN_POINT('',(0.173205080756888,-0.8,0.3));
#10481=CARTESIAN_POINT('',(-0.173205080756888,-1.28,0.3));
#10482=CARTESIAN_POINT('Origin',(0.346410161513775,-0.8,0.));
#10483=CARTESIAN_POINT('',(0.173205080756888,-0.8,0.3));
#10484=CARTESIAN_POINT('',(0.173205080756888,-1.28,0.3));
#10485=CARTESIAN_POINT('Origin',(0.,-0.8,-5.55111512312578E-17));
#10486=CARTESIAN_POINT('Origin',(0.,-1.28,-5.55111512312578E-17));
#10487=CARTESIAN_POINT('Origin',(0.,-2.5,0.));
#10488=CARTESIAN_POINT('',(-0.3933,-2.5,4.81653586104654E-17));
#10489=CARTESIAN_POINT('Origin',(0.,-2.5,0.));
#10490=CARTESIAN_POINT('Origin',(0.6,0.8,0.));
#10491=CARTESIAN_POINT('',(-0.6,0.8,-7.34788079488412E-17));
#10492=CARTESIAN_POINT('Origin',(0.,0.8,0.));
#10493=CARTESIAN_POINT('Origin',(0.,0.775,0.));
#10494=CARTESIAN_POINT('',(-0.65,0.75,-7.9602041944578E-17));
#10495=CARTESIAN_POINT('Origin',(0.,0.75,0.));
#10496=CARTESIAN_POINT('',(-0.625,0.775,-7.65404249467096E-17));
#10497=CARTESIAN_POINT('Origin',(0.,0.39,0.));
#10498=CARTESIAN_POINT('',(-0.65,0.0299999999999998,-7.9602041944578E-17));
#10499=CARTESIAN_POINT('Origin',(0.,0.0299999999999998,0.));
#10500=CARTESIAN_POINT('',(-0.65,0.39,-7.9602041944578E-17));
#10501=CARTESIAN_POINT('Origin',(0.,0.0150000000000001,0.));
#10502=CARTESIAN_POINT('',(-0.62,5.89805981832114E-17,-7.59281015471359E-17));
#10503=CARTESIAN_POINT('Origin',(0.,0.,0.));
#10504=CARTESIAN_POINT('',(-0.635,0.0150000000000001,-7.77650717458569E-17));
#10505=CARTESIAN_POINT('Origin',(0.42,0.,0.));
#10506=CARTESIAN_POINT('',(-0.42,-3.46944695195361E-18,-5.14351655641888E-17));
#10507=CARTESIAN_POINT('Origin',(0.,0.,0.));
#10508=CARTESIAN_POINT('Origin',(0.,-0.02,0.));
#10509=CARTESIAN_POINT('',(-0.3933,-0.0534000000000001,4.81653586104654E-17));
#10510=CARTESIAN_POINT('Origin',(0.,-0.0534000000000001,0.));
#10511=CARTESIAN_POINT('',(-0.41,-0.02,-5.02105187650415E-17));
#10512=CARTESIAN_POINT('Origin',(0.,-1.48,0.));
#10513=CARTESIAN_POINT('',(-0.3933,-1.48,-4.81653586104654E-17));
#10514=CARTESIAN_POINT('',(0.,0.,0.));
#10515=CARTESIAN_POINT('Origin',(0.0866025403784439,-0.4,-0.15));
#10516=CARTESIAN_POINT('',(0.173205080756888,-0.4,0.));
#10517=CARTESIAN_POINT('',(0.0866025403784439,-0.4,-0.15));
#10518=CARTESIAN_POINT('',(0.173205080756888,-0.4,0.));
#10519=CARTESIAN_POINT('',(0.0866025403784439,-0.64,-0.15));
#10520=CARTESIAN_POINT('',(0.0866025403784439,-0.4,-0.15));
#10521=CARTESIAN_POINT('',(0.173205080756888,-0.64,0.));
#10522=CARTESIAN_POINT('',(0.173205080756888,-0.64,0.));
#10523=CARTESIAN_POINT('',(0.173205080756888,-0.4,0.));
#10524=CARTESIAN_POINT('Origin',(-0.0866025403784438,-0.4,-0.15));
#10525=CARTESIAN_POINT('',(-0.0866025403784438,-0.4,-0.15));
#10526=CARTESIAN_POINT('',(0.0866025403784439,-0.4,-0.15));
#10527=CARTESIAN_POINT('',(-0.0866025403784438,-0.64,-0.15));
#10528=CARTESIAN_POINT('',(-0.0866025403784438,-0.4,-0.15));
#10529=CARTESIAN_POINT('',(0.0866025403784439,-0.64,-0.15));
#10530=CARTESIAN_POINT('Origin',(-0.173205080756888,-0.4,-2.77555756156289E-17));
#10531=CARTESIAN_POINT('',(-0.173205080756888,-0.4,-2.12115047744981E-17));
#10532=CARTESIAN_POINT('',(-0.0866025403784438,-0.4,-0.15));
#10533=CARTESIAN_POINT('',(-0.173205080756888,-0.64,-2.77555756156289E-17));
#10534=CARTESIAN_POINT('',(-0.173205080756888,-0.4,-2.12115047744981E-17));
#10535=CARTESIAN_POINT('',(-0.0866025403784438,-0.64,-0.15));
#10536=CARTESIAN_POINT('Origin',(-0.0866025403784439,-0.4,0.15));
#10537=CARTESIAN_POINT('',(-0.0866025403784439,-0.4,0.15));
#10538=CARTESIAN_POINT('',(-0.173205080756888,-0.4,-2.12115047744981E-17));
#10539=CARTESIAN_POINT('',(-0.0866025403784439,-0.64,0.15));
#10540=CARTESIAN_POINT('',(-0.0866025403784439,-0.4,0.15));
#10541=CARTESIAN_POINT('',(-0.173205080756888,-0.64,-2.12115047744981E-17));
#10542=CARTESIAN_POINT('Origin',(0.0866025403784439,-0.4,0.15));
#10543=CARTESIAN_POINT('',(0.0866025403784439,-0.4,0.15));
#10544=CARTESIAN_POINT('',(-0.0866025403784439,-0.4,0.15));
#10545=CARTESIAN_POINT('',(0.0866025403784439,-0.64,0.15));
#10546=CARTESIAN_POINT('',(0.0866025403784439,-0.4,0.15));
#10547=CARTESIAN_POINT('',(-0.0866025403784439,-0.64,0.15));
#10548=CARTESIAN_POINT('Origin',(0.173205080756888,-0.4,0.));
#10549=CARTESIAN_POINT('',(0.0866025403784439,-0.4,0.15));
#10550=CARTESIAN_POINT('',(0.0866025403784439,-0.64,0.15));
#10551=CARTESIAN_POINT('Origin',(0.,-0.4,-2.77555756156289E-17));
#10552=CARTESIAN_POINT('Origin',(0.,-0.64,-2.77555756156289E-17));
#10553=CARTESIAN_POINT('Origin',(0.,-1.,0.));
#10554=CARTESIAN_POINT('',(-0.1954,-1.,2.39295984553393E-17));
#10555=CARTESIAN_POINT('Origin',(0.,-1.,0.));
#10556=CARTESIAN_POINT('Origin',(0.3,0.4,0.));
#10557=CARTESIAN_POINT('',(-0.3,0.4,-3.67394039744206E-17));
#10558=CARTESIAN_POINT('Origin',(0.,0.4,0.));
#10559=CARTESIAN_POINT('Origin',(0.,0.375,0.));
#10560=CARTESIAN_POINT('',(-0.35,0.35,-4.28626379701573E-17));
#10561=CARTESIAN_POINT('Origin',(0.,0.35,0.));
#10562=CARTESIAN_POINT('',(-0.325,0.375,-3.9801020972289E-17));
#10563=CARTESIAN_POINT('Origin',(0.,0.19,0.));
#10564=CARTESIAN_POINT('',(-0.35,0.03,-4.28626379701574E-17));
#10565=CARTESIAN_POINT('Origin',(0.,0.03,0.));
#10566=CARTESIAN_POINT('',(-0.35,0.19,-4.28626379701574E-17));
#10567=CARTESIAN_POINT('Origin',(0.,0.0149999999999999,0.));
#10568=CARTESIAN_POINT('',(-0.32,-3.29597460435593E-17,-3.91886975727153E-17));
#10569=CARTESIAN_POINT('Origin',(0.,0.,0.));
#10570=CARTESIAN_POINT('',(-0.335,0.0149999999999999,-4.10256677714363E-17));
#10571=CARTESIAN_POINT('Origin',(0.22,0.,0.));
#10572=CARTESIAN_POINT('',(-0.22,-6.93889390390723E-18,-2.69422295812418E-17));
#10573=CARTESIAN_POINT('Origin',(0.,0.,0.));
#10574=CARTESIAN_POINT('Origin',(0.,-0.02,0.));
#10575=CARTESIAN_POINT('',(-0.1954,-0.0492,2.39295984553393E-17));
#10576=CARTESIAN_POINT('Origin',(0.,-0.0492,0.));
#10577=CARTESIAN_POINT('',(-0.21,-0.02,-2.57175827820944E-17));
#10578=CARTESIAN_POINT('Origin',(0.,-0.8,0.));
#10579=CARTESIAN_POINT('',(-0.1954,-0.8,-2.39295984553393E-17));
#10580=CARTESIAN_POINT('',(0.,0.,0.));
#10581=CARTESIAN_POINT('',(0.,0.,0.));
#10582=CARTESIAN_POINT('Origin',(0.,-7.,6.53));
#10583=CARTESIAN_POINT('',(-1.,20.,6.53));
#10584=CARTESIAN_POINT('Origin',(0.,20.,6.53));
#10585=CARTESIAN_POINT('',(-1.,-7.,6.53));
#10586=CARTESIAN_POINT('',(-1.,-7.,6.53));
#10587=CARTESIAN_POINT('Origin',(0.,-7.,6.53));
#10588=CARTESIAN_POINT('Origin',(0.,20.,6.53));
#10589=CARTESIAN_POINT('Origin',(0.,-7.,6.53));
#10590=CARTESIAN_POINT('',(0.,0.,0.));
#10591=CARTESIAN_POINT('Origin',(0.,-1.25,7.52));
#10592=CARTESIAN_POINT('',(0.172988438920056,-1.36905880899792,7.52));
#10593=CARTESIAN_POINT('',(0.172988438920056,-1.13094119100209,7.52));
#10594=CARTESIAN_POINT('',(0.172988438920056,-1.65,7.52));
#10595=CARTESIAN_POINT('Origin',(0.,-1.25,7.52));
#10596=CARTESIAN_POINT('Origin',(0.,-1.25,7.52));
#10597=CARTESIAN_POINT('',(-0.172988438920056,-1.36905880899792,7.52));
#10598=CARTESIAN_POINT('Ctrl Pts',(-0.172988438920056,-1.36905880899792,
7.52));
#10599=CARTESIAN_POINT('Ctrl Pts',(-0.165594865311314,-1.37980142239529,
7.52129192197638));
#10600=CARTESIAN_POINT('Ctrl Pts',(-0.157297138725606,-1.38968770937274,
7.52265394943905));
#10601=CARTESIAN_POINT('Ctrl Pts',(-0.129892073845076,-1.41709277425327,
7.5267480843909));
#10602=CARTESIAN_POINT('Ctrl Pts',(-0.106330167759284,-1.43324205633295,
7.52969589327638));
#10603=CARTESIAN_POINT('Ctrl Pts',(-0.0546129046324105,-1.45469779396491,
7.53385029472357));
#10604=CARTESIAN_POINT('Ctrl Pts',(-0.0264512308298517,-1.46,7.535));
#10605=CARTESIAN_POINT('Ctrl Pts',(0.0264512308298516,-1.46,7.535));
#10606=CARTESIAN_POINT('Ctrl Pts',(0.0546129046324104,-1.45469779396491,
7.53385029472357));
#10607=CARTESIAN_POINT('Ctrl Pts',(0.106330167759284,-1.43324205633295,
7.52969589327638));
#10608=CARTESIAN_POINT('Ctrl Pts',(0.129892073845076,-1.41709277425327,
7.5267480843909));
#10609=CARTESIAN_POINT('Ctrl Pts',(0.157297138725606,-1.38968770937274,
7.52265394943905));
#10610=CARTESIAN_POINT('Ctrl Pts',(0.165594865311315,-1.37980142239529,
7.52129192197638));
#10611=CARTESIAN_POINT('Ctrl Pts',(0.172988438920056,-1.36905880899792,
7.52));
#10612=CARTESIAN_POINT('',(-0.21,-1.25,7.52));
#10613=CARTESIAN_POINT('Origin',(0.,-1.25,7.52));
#10614=CARTESIAN_POINT('',(-0.21,-1.25,8.01522725533839));
#10615=CARTESIAN_POINT('',(-0.21,-1.25,7.52));
#10616=CARTESIAN_POINT('',(0.21,-1.25,8.01522725533839));
#10617=CARTESIAN_POINT('Ctrl Pts',(0.21,-1.25,8.01522725533839));
#10618=CARTESIAN_POINT('Ctrl Pts',(0.21,-1.27640552692445,8.01522725533839));
#10619=CARTESIAN_POINT('Ctrl Pts',(0.204715737269596,-1.30454707409071,
8.01600415954412));
#10620=CARTESIAN_POINT('Ctrl Pts',(0.183273763036332,-1.35627626890513,
8.01880073282317));
#10621=CARTESIAN_POINT('Ctrl Pts',(0.167117923970394,-1.37986692412796,
8.02077897157582));
#10622=CARTESIAN_POINT('Ctrl Pts',(0.129867169887369,-1.41711767821098,
8.02448481141327));
#10623=CARTESIAN_POINT('Ctrl Pts',(0.106276408305765,-1.43327371000135,
8.02645455657129));
#10624=CARTESIAN_POINT('Ctrl Pts',(0.0545468514059001,-1.45471582482622,
8.02923165515645));
#10625=CARTESIAN_POINT('Ctrl Pts',(0.0264051785092814,-1.46,8.03));
#10626=CARTESIAN_POINT('Ctrl Pts',(-0.0264051785092814,-1.46,8.03));
#10627=CARTESIAN_POINT('Ctrl Pts',(-0.0545468514059,-1.45471582482622,8.02923165515645));
#10628=CARTESIAN_POINT('Ctrl Pts',(-0.106276408305765,-1.43327371000135,
8.02645455657129));
#10629=CARTESIAN_POINT('Ctrl Pts',(-0.129867169887369,-1.41711767821098,
8.02448481141327));
#10630=CARTESIAN_POINT('Ctrl Pts',(-0.167117923970394,-1.37986692412796,
8.02077897157582));
#10631=CARTESIAN_POINT('Ctrl Pts',(-0.183273763036331,-1.35627626890513,
8.01880073282317));
#10632=CARTESIAN_POINT('Ctrl Pts',(-0.204715737269596,-1.30454707409071,
8.01600415954412));
#10633=CARTESIAN_POINT('Ctrl Pts',(-0.21,-1.27640552692445,8.01522725533839));
#10634=CARTESIAN_POINT('Ctrl Pts',(-0.21,-1.25,8.01522725533839));
#10635=CARTESIAN_POINT('Ctrl Pts',(-0.21,-1.25,8.01522725533839));
#10636=CARTESIAN_POINT('Ctrl Pts',(-0.21,-1.22359447307555,8.01522725533839));
#10637=CARTESIAN_POINT('Ctrl Pts',(-0.204715737269596,-1.19545292590929,
8.01600415954412));
#10638=CARTESIAN_POINT('Ctrl Pts',(-0.183273763036332,-1.14372373109487,
8.01880073282317));
#10639=CARTESIAN_POINT('Ctrl Pts',(-0.167117923970394,-1.12013307587204,
8.02077897157582));
#10640=CARTESIAN_POINT('Ctrl Pts',(-0.129867169887369,-1.08288232178902,
8.02448481141327));
#10641=CARTESIAN_POINT('Ctrl Pts',(-0.106276408305765,-1.06672628999865,
8.02645455657129));
#10642=CARTESIAN_POINT('Ctrl Pts',(-0.0545468514059001,-1.04528417517378,
8.02923165515645));
#10643=CARTESIAN_POINT('Ctrl Pts',(-0.0264051785092814,-1.04,8.03));
#10644=CARTESIAN_POINT('Ctrl Pts',(0.0264051785092814,-1.04,8.03));
#10645=CARTESIAN_POINT('Ctrl Pts',(0.0545468514059002,-1.04528417517378,
8.02923165515645));
#10646=CARTESIAN_POINT('Ctrl Pts',(0.106276408305765,-1.06672628999865,
8.02645455657129));
#10647=CARTESIAN_POINT('Ctrl Pts',(0.129867169887369,-1.08288232178902,
8.02448481141327));
#10648=CARTESIAN_POINT('Ctrl Pts',(0.167117923970394,-1.12013307587204,
8.02077897157582));
#10649=CARTESIAN_POINT('Ctrl Pts',(0.183273763036331,-1.14372373109487,
8.01880073282317));
#10650=CARTESIAN_POINT('Ctrl Pts',(0.204715737269596,-1.19545292590929,
8.01600415954412));
#10651=CARTESIAN_POINT('Ctrl Pts',(0.21,-1.22359447307555,8.01522725533839));
#10652=CARTESIAN_POINT('Ctrl Pts',(0.21,-1.25,8.01522725533839));
#10653=CARTESIAN_POINT('',(-0.172988438920056,-1.13094119100209,7.52));
#10654=CARTESIAN_POINT('Origin',(0.,-1.25,7.52));
#10655=CARTESIAN_POINT('Ctrl Pts',(0.172988438920056,-1.13094119100209,
7.52));
#10656=CARTESIAN_POINT('Ctrl Pts',(0.165594865311315,-1.12019857760471,
7.52129192197638));
#10657=CARTESIAN_POINT('Ctrl Pts',(0.157297138725606,-1.11031229062726,
7.52265394943905));
#10658=CARTESIAN_POINT('Ctrl Pts',(0.129892073845076,-1.08290722574673,
7.5267480843909));
#10659=CARTESIAN_POINT('Ctrl Pts',(0.106330167759284,-1.06675794366705,
7.52969589327638));
#10660=CARTESIAN_POINT('Ctrl Pts',(0.0546129046324104,-1.04530220603509,
7.53385029472357));
#10661=CARTESIAN_POINT('Ctrl Pts',(0.0264512308298516,-1.04,7.535));
#10662=CARTESIAN_POINT('Ctrl Pts',(-0.0264512308298516,-1.04,7.535));
#10663=CARTESIAN_POINT('Ctrl Pts',(-0.0546129046324104,-1.04530220603509,
7.53385029472357));
#10664=CARTESIAN_POINT('Ctrl Pts',(-0.106330167759284,-1.06675794366705,
7.52969589327638));
#10665=CARTESIAN_POINT('Ctrl Pts',(-0.129892073845076,-1.08290722574673,
7.5267480843909));
#10666=CARTESIAN_POINT('Ctrl Pts',(-0.157297138725606,-1.11031229062726,
7.52265394943905));
#10667=CARTESIAN_POINT('Ctrl Pts',(-0.165594865311315,-1.12019857760471,
7.52129192197638));
#10668=CARTESIAN_POINT('Ctrl Pts',(-0.172988438920056,-1.13094119100209,
7.52));
#10669=CARTESIAN_POINT('Origin',(0.,-1.25,7.52));
#10670=CARTESIAN_POINT('',(-0.172988438920056,-1.65,7.52));
#10671=CARTESIAN_POINT('Origin',(0.,-1.65,6.53));
#10672=CARTESIAN_POINT('',(-1.005,-0.85,6.53));
#10673=CARTESIAN_POINT('Origin',(0.,-0.85,6.53));
#10674=CARTESIAN_POINT('',(-1.005,-1.65,6.53));
#10675=CARTESIAN_POINT('',(-1.005,-1.65,6.53));
#10676=CARTESIAN_POINT('Origin',(0.,-1.65,6.53));
#10677=CARTESIAN_POINT('Origin',(0.,-1.65,6.53));
#10678=CARTESIAN_POINT('',(-1.5,-0.85,6.53));
#10679=CARTESIAN_POINT('Origin',(0.,-0.85,6.53));
#10680=CARTESIAN_POINT('',(-1.5,-1.65,6.53));
#10681=CARTESIAN_POINT('',(-1.5,-1.65,6.53));
#10682=CARTESIAN_POINT('Origin',(0.,-1.65,6.53));
#10683=CARTESIAN_POINT('Origin',(0.,-0.85,6.53));
#10684=CARTESIAN_POINT('Origin',(0.,-1.65,6.53));
#10685=CARTESIAN_POINT('',(0.,0.,0.));
#10686=CARTESIAN_POINT('Origin',(0.,18.85,7.52));
#10687=CARTESIAN_POINT('',(0.172988438920056,18.7309411910021,7.52));
#10688=CARTESIAN_POINT('',(0.172988438920056,18.9690588089979,7.52));
#10689=CARTESIAN_POINT('',(0.172988438920056,18.45,7.52));
#10690=CARTESIAN_POINT('Origin',(0.,18.85,7.52));
#10691=CARTESIAN_POINT('Origin',(0.,18.85,7.52));
#10692=CARTESIAN_POINT('',(-0.172988438920056,18.7309411910021,7.52));
#10693=CARTESIAN_POINT('Ctrl Pts',(-0.172988438920055,18.7309411910021,
7.52));
#10694=CARTESIAN_POINT('Ctrl Pts',(-0.165594865311313,18.7201985776047,
7.52129192197638));
#10695=CARTESIAN_POINT('Ctrl Pts',(-0.157297138725605,18.7103122906273,
7.52265394943905));
#10696=CARTESIAN_POINT('Ctrl Pts',(-0.129892073845076,18.6829072257467,
7.5267480843909));
#10697=CARTESIAN_POINT('Ctrl Pts',(-0.106330167759285,18.6667579436671,
7.52969589327637));
#10698=CARTESIAN_POINT('Ctrl Pts',(-0.0546129046324106,18.6453022060351,
7.53385029472357));
#10699=CARTESIAN_POINT('Ctrl Pts',(-0.0264512308298518,18.64,7.535));
#10700=CARTESIAN_POINT('Ctrl Pts',(0.0264512308298517,18.64,7.535));
#10701=CARTESIAN_POINT('Ctrl Pts',(0.0546129046324104,18.6453022060351,
7.53385029472357));
#10702=CARTESIAN_POINT('Ctrl Pts',(0.106330167759284,18.6667579436671,7.52969589327638));
#10703=CARTESIAN_POINT('Ctrl Pts',(0.129892073845076,18.6829072257467,7.5267480843909));
#10704=CARTESIAN_POINT('Ctrl Pts',(0.157297138725605,18.7103122906273,7.52265394943905));
#10705=CARTESIAN_POINT('Ctrl Pts',(0.165594865311314,18.7201985776047,7.52129192197638));
#10706=CARTESIAN_POINT('Ctrl Pts',(0.172988438920056,18.7309411910021,7.52));
#10707=CARTESIAN_POINT('',(-0.21,18.85,7.52));
#10708=CARTESIAN_POINT('Origin',(0.,18.85,7.52));
#10709=CARTESIAN_POINT('',(-0.21,18.85,8.01522725533839));
#10710=CARTESIAN_POINT('',(-0.21,18.85,7.52));
#10711=CARTESIAN_POINT('',(0.21,18.85,8.01522725533839));
#10712=CARTESIAN_POINT('Ctrl Pts',(0.21,18.85,8.01522725533839));
#10713=CARTESIAN_POINT('Ctrl Pts',(0.21,18.8235944730755,8.01522725533839));
#10714=CARTESIAN_POINT('Ctrl Pts',(0.204715737269595,18.7954529259093,8.01600415954412));
#10715=CARTESIAN_POINT('Ctrl Pts',(0.18327376303633,18.7437237310949,8.01880073282317));
#10716=CARTESIAN_POINT('Ctrl Pts',(0.167117923970393,18.720133075872,8.02077897157582));
#10717=CARTESIAN_POINT('Ctrl Pts',(0.129867169887369,18.682882321789,8.02448481141327));
#10718=CARTESIAN_POINT('Ctrl Pts',(0.106276408305767,18.6667262899986,8.02645455657129));
#10719=CARTESIAN_POINT('Ctrl Pts',(0.0545468514059018,18.6452841751738,
8.02923165515645));
#10720=CARTESIAN_POINT('Ctrl Pts',(0.0264051785092816,18.64,8.03));
#10721=CARTESIAN_POINT('Ctrl Pts',(-0.0264051785092815,18.64,8.03));
#10722=CARTESIAN_POINT('Ctrl Pts',(-0.0545468514059018,18.6452841751738,
8.02923165515645));
#10723=CARTESIAN_POINT('Ctrl Pts',(-0.106276408305767,18.6667262899986,
8.02645455657129));
#10724=CARTESIAN_POINT('Ctrl Pts',(-0.129867169887368,18.682882321789,8.02448481141327));
#10725=CARTESIAN_POINT('Ctrl Pts',(-0.167117923970393,18.720133075872,8.02077897157582));
#10726=CARTESIAN_POINT('Ctrl Pts',(-0.18327376303633,18.7437237310949,8.01880073282317));
#10727=CARTESIAN_POINT('Ctrl Pts',(-0.204715737269595,18.7954529259093,
8.01600415954412));
#10728=CARTESIAN_POINT('Ctrl Pts',(-0.21,18.8235944730755,8.01522725533839));
#10729=CARTESIAN_POINT('Ctrl Pts',(-0.21,18.85,8.01522725533839));
#10730=CARTESIAN_POINT('Ctrl Pts',(-0.21,18.85,8.01522725533839));
#10731=CARTESIAN_POINT('Ctrl Pts',(-0.21,18.8764055269245,8.01522725533839));
#10732=CARTESIAN_POINT('Ctrl Pts',(-0.204715737269595,18.9045470740907,
8.01600415954412));
#10733=CARTESIAN_POINT('Ctrl Pts',(-0.18327376303633,18.9562762689051,8.01880073282317));
#10734=CARTESIAN_POINT('Ctrl Pts',(-0.167117923970393,18.979866924128,8.02077897157582));
#10735=CARTESIAN_POINT('Ctrl Pts',(-0.129867169887369,19.017117678211,8.02448481141327));
#10736=CARTESIAN_POINT('Ctrl Pts',(-0.106276408305767,19.0332737100014,
8.02645455657129));
#10737=CARTESIAN_POINT('Ctrl Pts',(-0.0545468514059018,19.0547158248262,
8.02923165515645));
#10738=CARTESIAN_POINT('Ctrl Pts',(-0.0264051785092816,19.06,8.03));
#10739=CARTESIAN_POINT('Ctrl Pts',(0.0264051785092815,19.06,8.03));
#10740=CARTESIAN_POINT('Ctrl Pts',(0.0545468514059019,19.0547158248262,
8.02923165515645));
#10741=CARTESIAN_POINT('Ctrl Pts',(0.106276408305767,19.0332737100014,8.02645455657129));
#10742=CARTESIAN_POINT('Ctrl Pts',(0.129867169887368,19.017117678211,8.02448481141327));
#10743=CARTESIAN_POINT('Ctrl Pts',(0.167117923970393,18.979866924128,8.02077897157582));
#10744=CARTESIAN_POINT('Ctrl Pts',(0.18327376303633,18.9562762689051,8.01880073282317));
#10745=CARTESIAN_POINT('Ctrl Pts',(0.204715737269595,18.9045470740907,8.01600415954412));
#10746=CARTESIAN_POINT('Ctrl Pts',(0.21,18.8764055269245,8.01522725533839));
#10747=CARTESIAN_POINT('Ctrl Pts',(0.21,18.85,8.01522725533839));
#10748=CARTESIAN_POINT('',(-0.172988438920056,18.9690588089979,7.52));
#10749=CARTESIAN_POINT('Origin',(0.,18.85,7.52));
#10750=CARTESIAN_POINT('Ctrl Pts',(0.172988438920053,18.9690588089979,7.52));
#10751=CARTESIAN_POINT('Ctrl Pts',(0.165594865311312,18.9798014223953,7.52129192197638));
#10752=CARTESIAN_POINT('Ctrl Pts',(0.157297138725604,18.9896877093727,7.52265394943905));
#10753=CARTESIAN_POINT('Ctrl Pts',(0.129892073845076,19.0170927742533,7.5267480843909));
#10754=CARTESIAN_POINT('Ctrl Pts',(0.106330167759284,19.033242056333,7.52969589327638));
#10755=CARTESIAN_POINT('Ctrl Pts',(0.0546129046324105,19.0546977939649,
7.53385029472357));
#10756=CARTESIAN_POINT('Ctrl Pts',(0.0264512308298518,19.06,7.535));
#10757=CARTESIAN_POINT('Ctrl Pts',(-0.0264512308298517,19.06,7.535));
#10758=CARTESIAN_POINT('Ctrl Pts',(-0.0546129046324105,19.0546977939649,
7.53385029472357));
#10759=CARTESIAN_POINT('Ctrl Pts',(-0.106330167759284,19.033242056333,7.52969589327638));
#10760=CARTESIAN_POINT('Ctrl Pts',(-0.129892073845076,19.0170927742533,
7.5267480843909));
#10761=CARTESIAN_POINT('Ctrl Pts',(-0.157297138725604,18.9896877093727,
7.52265394943905));
#10762=CARTESIAN_POINT('Ctrl Pts',(-0.165594865311312,18.9798014223953,
7.52129192197638));
#10763=CARTESIAN_POINT('Ctrl Pts',(-0.172988438920053,18.9690588089979,
7.52));
#10764=CARTESIAN_POINT('Origin',(0.,18.85,7.52));
#10765=CARTESIAN_POINT('',(-0.172988438920056,18.45,7.52));
#10766=CARTESIAN_POINT('Origin',(0.,18.45,6.53));
#10767=CARTESIAN_POINT('',(-1.005,19.25,6.53));
#10768=CARTESIAN_POINT('Origin',(0.,19.25,6.53));
#10769=CARTESIAN_POINT('',(-1.005,18.45,6.53));
#10770=CARTESIAN_POINT('',(-1.005,18.45,6.53));
#10771=CARTESIAN_POINT('Origin',(0.,18.45,6.53));
#10772=CARTESIAN_POINT('Origin',(0.,18.45,6.53));
#10773=CARTESIAN_POINT('',(-1.5,19.25,6.53));
#10774=CARTESIAN_POINT('Origin',(0.,19.25,6.53));
#10775=CARTESIAN_POINT('',(-1.5,18.45,6.53));
#10776=CARTESIAN_POINT('',(-1.5,18.45,6.53));
#10777=CARTESIAN_POINT('Origin',(0.,18.45,6.53));
#10778=CARTESIAN_POINT('Origin',(0.,19.25,6.53));
#10779=CARTESIAN_POINT('Origin',(0.,18.45,6.53));
#10780=CARTESIAN_POINT('',(0.,0.,0.));
#10781=CARTESIAN_POINT('Origin',(0.,3.,6.53));
#10782=CARTESIAN_POINT('',(-3.6,13.,6.53));
#10783=CARTESIAN_POINT('Origin',(0.,13.,6.53));
#10784=CARTESIAN_POINT('',(-3.6,3.,6.53));
#10785=CARTESIAN_POINT('',(-3.6,3.,6.53));
#10786=CARTESIAN_POINT('Origin',(0.,3.,6.53));
#10787=CARTESIAN_POINT('Origin',(0.,3.,6.53));
#10788=CARTESIAN_POINT('',(-4.,13.,6.53));
#10789=CARTESIAN_POINT('Origin',(0.,13.,6.53));
#10790=CARTESIAN_POINT('',(-4.,3.,6.53));
#10791=CARTESIAN_POINT('',(-4.,3.,6.53));
#10792=CARTESIAN_POINT('Origin',(0.,3.,6.53));
#10793=CARTESIAN_POINT('Origin',(0.,13.,6.53));
#10794=CARTESIAN_POINT('Origin',(0.,3.,6.53));
#10795=CARTESIAN_POINT('',(0.,0.,0.));
#10796=CARTESIAN_POINT('Origin',(0.,2.6,6.53));
#10797=CARTESIAN_POINT('',(-1.005,3.,6.53));
#10798=CARTESIAN_POINT('Origin',(0.,3.,6.53));
#10799=CARTESIAN_POINT('',(-1.005,2.6,6.53));
#10800=CARTESIAN_POINT('',(-1.005,2.6,6.53));
#10801=CARTESIAN_POINT('Origin',(0.,2.6,6.53));
#10802=CARTESIAN_POINT('Origin',(0.,2.6,6.53));
#10803=CARTESIAN_POINT('',(-4.5,3.,6.53));
#10804=CARTESIAN_POINT('Origin',(0.,3.,6.53));
#10805=CARTESIAN_POINT('',(-4.5,2.6,6.53));
#10806=CARTESIAN_POINT('',(-4.5,2.6,6.53));
#10807=CARTESIAN_POINT('Origin',(0.,2.6,6.53));
#10808=CARTESIAN_POINT('Origin',(0.,3.,6.53));
#10809=CARTESIAN_POINT('Origin',(0.,2.6,6.53));
#10810=CARTESIAN_POINT('',(0.,0.,0.));
#10811=CARTESIAN_POINT('Origin',(0.,3.5,7.52));
#10812=CARTESIAN_POINT('',(0.172988438920056,3.38094119100209,7.52));
#10813=CARTESIAN_POINT('',(0.172988438920056,3.61905880899792,7.52));
#10814=CARTESIAN_POINT('',(0.172988438920056,3.,7.52));
#10815=CARTESIAN_POINT('Origin',(0.,3.5,7.52));
#10816=CARTESIAN_POINT('Origin',(0.,3.5,7.52));
#10817=CARTESIAN_POINT('',(-0.172988438920056,3.38094119100209,7.52));
#10818=CARTESIAN_POINT('Ctrl Pts',(-0.172988438920056,3.38094119100209,
7.52));
#10819=CARTESIAN_POINT('Ctrl Pts',(-0.165594865311315,3.37019857760471,
7.52129192197638));
#10820=CARTESIAN_POINT('Ctrl Pts',(-0.157297138725606,3.36031229062726,
7.52265394943905));
#10821=CARTESIAN_POINT('Ctrl Pts',(-0.129892073845076,3.33290722574673,
7.5267480843909));
#10822=CARTESIAN_POINT('Ctrl Pts',(-0.106330167759285,3.31675794366705,
7.52969589327638));
#10823=CARTESIAN_POINT('Ctrl Pts',(-0.0546129046324106,3.29530220603509,
7.53385029472357));
#10824=CARTESIAN_POINT('Ctrl Pts',(-0.0264512308298517,3.29,7.535));
#10825=CARTESIAN_POINT('Ctrl Pts',(0.0264512308298516,3.29,7.535));
#10826=CARTESIAN_POINT('Ctrl Pts',(0.0546129046324105,3.29530220603509,
7.53385029472357));
#10827=CARTESIAN_POINT('Ctrl Pts',(0.106330167759284,3.31675794366705,7.52969589327638));
#10828=CARTESIAN_POINT('Ctrl Pts',(0.129892073845076,3.33290722574673,7.5267480843909));
#10829=CARTESIAN_POINT('Ctrl Pts',(0.157297138725606,3.36031229062726,7.52265394943905));
#10830=CARTESIAN_POINT('Ctrl Pts',(0.165594865311315,3.37019857760471,7.52129192197638));
#10831=CARTESIAN_POINT('Ctrl Pts',(0.172988438920056,3.38094119100209,7.52));
#10832=CARTESIAN_POINT('',(-0.21,3.5,7.52));
#10833=CARTESIAN_POINT('Origin',(0.,3.5,7.52));
#10834=CARTESIAN_POINT('',(-0.21,3.5,8.11615888233178));
#10835=CARTESIAN_POINT('',(-0.21,3.5,7.52));
#10836=CARTESIAN_POINT('',(0.21,3.5,8.11615888233178));
#10837=CARTESIAN_POINT('Ctrl Pts',(0.21,3.5,8.11615888233178));
#10838=CARTESIAN_POINT('Ctrl Pts',(0.21,3.47359906579625,8.11615888233178));
#10839=CARTESIAN_POINT('Ctrl Pts',(0.20471752266132,3.44545944463489,8.11688606295397));
#10840=CARTESIAN_POINT('Ctrl Pts',(0.183276841782292,3.3937289476995,8.11950502964782));
#10841=CARTESIAN_POINT('Ctrl Pts',(0.167120287247804,3.37013543914945,8.12135816887013));
#10842=CARTESIAN_POINT('Ctrl Pts',(0.129864750292352,3.332879902194,8.12483075953278));
#10843=CARTESIAN_POINT('Ctrl Pts',(0.106271159541076,3.31672319916877,8.12667690933009));
#10844=CARTESIAN_POINT('Ctrl Pts',(0.0545403836274688,3.2952824096556,8.12927985626981));
#10845=CARTESIAN_POINT('Ctrl Pts',(0.0264006657112965,3.29,8.13));
#10846=CARTESIAN_POINT('Ctrl Pts',(-0.0264006657112964,3.29,8.13));
#10847=CARTESIAN_POINT('Ctrl Pts',(-0.0545403836274688,3.2952824096556,
8.12927985626981));
#10848=CARTESIAN_POINT('Ctrl Pts',(-0.106271159541076,3.31672319916877,
8.12667690933009));
#10849=CARTESIAN_POINT('Ctrl Pts',(-0.129864750292352,3.332879902194,8.12483075953278));
#10850=CARTESIAN_POINT('Ctrl Pts',(-0.167120287247804,3.37013543914945,
8.12135816887013));
#10851=CARTESIAN_POINT('Ctrl Pts',(-0.183276841782292,3.3937289476995,8.11950502964782));
#10852=CARTESIAN_POINT('Ctrl Pts',(-0.20471752266132,3.44545944463489,8.11688606295397));
#10853=CARTESIAN_POINT('Ctrl Pts',(-0.21,3.47359906579625,8.11615888233178));
#10854=CARTESIAN_POINT('Ctrl Pts',(-0.21,3.5,8.11615888233178));
#10855=CARTESIAN_POINT('Ctrl Pts',(-0.21,3.5,8.11615888233178));
#10856=CARTESIAN_POINT('Ctrl Pts',(-0.21,3.52640093420375,8.11615888233178));
#10857=CARTESIAN_POINT('Ctrl Pts',(-0.20471752266132,3.55454055536511,8.11688606295397));
#10858=CARTESIAN_POINT('Ctrl Pts',(-0.183276841782292,3.6062710523005,8.11950502964782));
#10859=CARTESIAN_POINT('Ctrl Pts',(-0.167120287247804,3.62986456085055,
8.12135816887013));
#10860=CARTESIAN_POINT('Ctrl Pts',(-0.129864750292352,3.667120097806,8.12483075953278));
#10861=CARTESIAN_POINT('Ctrl Pts',(-0.106271159541076,3.68327680083123,
8.12667690933009));
#10862=CARTESIAN_POINT('Ctrl Pts',(-0.0545403836274688,3.7047175903444,
8.12927985626981));
#10863=CARTESIAN_POINT('Ctrl Pts',(-0.0264006657112965,3.71,8.13));
#10864=CARTESIAN_POINT('Ctrl Pts',(0.0264006657112965,3.71,8.13));
#10865=CARTESIAN_POINT('Ctrl Pts',(0.0545403836274689,3.7047175903444,8.12927985626981));
#10866=CARTESIAN_POINT('Ctrl Pts',(0.106271159541076,3.68327680083123,8.12667690933009));
#10867=CARTESIAN_POINT('Ctrl Pts',(0.129864750292352,3.667120097806,8.12483075953278));
#10868=CARTESIAN_POINT('Ctrl Pts',(0.167120287247804,3.62986456085055,8.12135816887013));
#10869=CARTESIAN_POINT('Ctrl Pts',(0.183276841782292,3.6062710523005,8.11950502964782));
#10870=CARTESIAN_POINT('Ctrl Pts',(0.20471752266132,3.55454055536511,8.11688606295397));
#10871=CARTESIAN_POINT('Ctrl Pts',(0.21,3.52640093420375,8.11615888233178));
#10872=CARTESIAN_POINT('Ctrl Pts',(0.21,3.5,8.11615888233178));
#10873=CARTESIAN_POINT('',(-0.172988438920056,3.61905880899792,7.52));
#10874=CARTESIAN_POINT('Origin',(0.,3.5,7.52));
#10875=CARTESIAN_POINT('Ctrl Pts',(0.172988438920056,3.61905880899792,7.52));
#10876=CARTESIAN_POINT('Ctrl Pts',(0.165594865311314,3.62980142239529,7.52129192197638));
#10877=CARTESIAN_POINT('Ctrl Pts',(0.157297138725606,3.63968770937274,7.52265394943905));
#10878=CARTESIAN_POINT('Ctrl Pts',(0.129892073845076,3.66709277425327,7.5267480843909));
#10879=CARTESIAN_POINT('Ctrl Pts',(0.106330167759284,3.68324205633295,7.52969589327638));
#10880=CARTESIAN_POINT('Ctrl Pts',(0.0546129046324106,3.70469779396491,
7.53385029472357));
#10881=CARTESIAN_POINT('Ctrl Pts',(0.0264512308298516,3.71,7.535));
#10882=CARTESIAN_POINT('Ctrl Pts',(-0.0264512308298516,3.71,7.535));
#10883=CARTESIAN_POINT('Ctrl Pts',(-0.0546129046324105,3.70469779396491,
7.53385029472357));
#10884=CARTESIAN_POINT('Ctrl Pts',(-0.106330167759284,3.68324205633295,
7.52969589327638));
#10885=CARTESIAN_POINT('Ctrl Pts',(-0.129892073845076,3.66709277425327,
7.5267480843909));
#10886=CARTESIAN_POINT('Ctrl Pts',(-0.157297138725606,3.63968770937274,
7.52265394943905));
#10887=CARTESIAN_POINT('Ctrl Pts',(-0.165594865311314,3.62980142239529,
7.52129192197638));
#10888=CARTESIAN_POINT('Ctrl Pts',(-0.172988438920056,3.61905880899792,
7.52));
#10889=CARTESIAN_POINT('Origin',(0.,3.5,7.52));
#10890=CARTESIAN_POINT('',(-0.172988438920056,3.,7.52));
#10891=CARTESIAN_POINT('Origin',(0.,3.,6.53));
#10892=CARTESIAN_POINT('',(-1.005,4.,6.53));
#10893=CARTESIAN_POINT('Origin',(0.,4.,6.53));
#10894=CARTESIAN_POINT('',(-1.005,3.,6.53));
#10895=CARTESIAN_POINT('',(-1.005,3.,6.53));
#10896=CARTESIAN_POINT('Origin',(0.,3.,6.53));
#10897=CARTESIAN_POINT('Origin',(0.,3.,6.53));
#10898=CARTESIAN_POINT('',(-1.6,4.,6.53));
#10899=CARTESIAN_POINT('Origin',(0.,4.,6.53));
#10900=CARTESIAN_POINT('',(-1.6,3.,6.53));
#10901=CARTESIAN_POINT('',(-1.6,3.,6.53));
#10902=CARTESIAN_POINT('Origin',(0.,3.,6.53));
#10903=CARTESIAN_POINT('Origin',(0.,4.,6.53));
#10904=CARTESIAN_POINT('Origin',(0.,3.,6.53));
#10905=CARTESIAN_POINT('',(0.,0.,0.));
#10906=CARTESIAN_POINT('Origin',(0.,13.,6.53));
#10907=CARTESIAN_POINT('',(-1.005,13.4,6.53));
#10908=CARTESIAN_POINT('Origin',(0.,13.4,6.53));
#10909=CARTESIAN_POINT('',(-1.005,13.,6.53));
#10910=CARTESIAN_POINT('',(-1.005,13.,6.53));
#10911=CARTESIAN_POINT('Origin',(0.,13.,6.53));
#10912=CARTESIAN_POINT('Origin',(0.,13.,6.53));
#10913=CARTESIAN_POINT('',(-4.5,13.4,6.53));
#10914=CARTESIAN_POINT('Origin',(0.,13.4,6.53));
#10915=CARTESIAN_POINT('',(-4.5,13.,6.53));
#10916=CARTESIAN_POINT('',(-4.5,13.,6.53));
#10917=CARTESIAN_POINT('Origin',(0.,13.,6.53));
#10918=CARTESIAN_POINT('Origin',(0.,13.4,6.53));
#10919=CARTESIAN_POINT('Origin',(0.,13.,6.53));
#10920=CARTESIAN_POINT('',(0.,0.,0.));
#10921=CARTESIAN_POINT('Origin',(0.,12.5,7.52));
#10922=CARTESIAN_POINT('',(0.172988438920056,12.3809411910021,7.52));
#10923=CARTESIAN_POINT('',(0.172988438920056,12.6190588089979,7.52));
#10924=CARTESIAN_POINT('',(0.172988438920056,12.,7.52));
#10925=CARTESIAN_POINT('Origin',(0.,12.5,7.52));
#10926=CARTESIAN_POINT('Origin',(0.,12.5,7.52));
#10927=CARTESIAN_POINT('',(-0.172988438920056,12.3809411910021,7.52));
#10928=CARTESIAN_POINT('Ctrl Pts',(-0.172988438920057,12.3809411910021,
7.52));
#10929=CARTESIAN_POINT('Ctrl Pts',(-0.165594865311316,12.3701985776047,
7.52129192197638));
#10930=CARTESIAN_POINT('Ctrl Pts',(-0.157297138725606,12.3603122906273,
7.52265394943905));
#10931=CARTESIAN_POINT('Ctrl Pts',(-0.129892073845076,12.3329072257467,
7.5267480843909));
#10932=CARTESIAN_POINT('Ctrl Pts',(-0.106330167759285,12.316757943667,7.52969589327638));
#10933=CARTESIAN_POINT('Ctrl Pts',(-0.0546129046324104,12.2953022060351,
7.53385029472357));
#10934=CARTESIAN_POINT('Ctrl Pts',(-0.0264512308298516,12.29,7.535));
#10935=CARTESIAN_POINT('Ctrl Pts',(0.0264512308298515,12.29,7.535));
#10936=CARTESIAN_POINT('Ctrl Pts',(0.0546129046324104,12.2953022060351,
7.53385029472357));
#10937=CARTESIAN_POINT('Ctrl Pts',(0.106330167759285,12.316757943667,7.52969589327638));
#10938=CARTESIAN_POINT('Ctrl Pts',(0.129892073845076,12.3329072257467,7.5267480843909));
#10939=CARTESIAN_POINT('Ctrl Pts',(0.157297138725607,12.3603122906273,7.52265394943905));
#10940=CARTESIAN_POINT('Ctrl Pts',(0.165594865311314,12.3701985776047,7.52129192197638));
#10941=CARTESIAN_POINT('Ctrl Pts',(0.172988438920056,12.3809411910021,7.52));
#10942=CARTESIAN_POINT('',(-0.21,12.5,7.52));
#10943=CARTESIAN_POINT('Origin',(0.,12.5,7.52));
#10944=CARTESIAN_POINT('',(-0.21,12.5,8.11615888233178));
#10945=CARTESIAN_POINT('',(-0.21,12.5,7.52));
#10946=CARTESIAN_POINT('',(0.21,12.5,8.11615888233178));
#10947=CARTESIAN_POINT('Ctrl Pts',(0.21,12.5,8.11615888233178));
#10948=CARTESIAN_POINT('Ctrl Pts',(0.21,12.4735990657963,8.11615888233178));
#10949=CARTESIAN_POINT('Ctrl Pts',(0.20471752266132,12.4454594446349,8.11688606295397));
#10950=CARTESIAN_POINT('Ctrl Pts',(0.183276841782292,12.3937289476995,8.11950502964782));
#10951=CARTESIAN_POINT('Ctrl Pts',(0.167120287247804,12.3701354391495,8.12135816887013));
#10952=CARTESIAN_POINT('Ctrl Pts',(0.129864750292352,12.332879902194,8.12483075953278));
#10953=CARTESIAN_POINT('Ctrl Pts',(0.106271159541075,12.3167231991688,8.12667690933009));
#10954=CARTESIAN_POINT('Ctrl Pts',(0.0545403836274679,12.2952824096556,
8.12927985626981));
#10955=CARTESIAN_POINT('Ctrl Pts',(0.0264006657112965,12.29,8.13));
#10956=CARTESIAN_POINT('Ctrl Pts',(-0.0264006657112964,12.29,8.13));
#10957=CARTESIAN_POINT('Ctrl Pts',(-0.0545403836274678,12.2952824096556,
8.12927985626981));
#10958=CARTESIAN_POINT('Ctrl Pts',(-0.106271159541075,12.3167231991688,
8.12667690933009));
#10959=CARTESIAN_POINT('Ctrl Pts',(-0.129864750292352,12.332879902194,8.12483075953278));
#10960=CARTESIAN_POINT('Ctrl Pts',(-0.167120287247804,12.3701354391495,
8.12135816887013));
#10961=CARTESIAN_POINT('Ctrl Pts',(-0.183276841782292,12.3937289476995,
8.11950502964782));
#10962=CARTESIAN_POINT('Ctrl Pts',(-0.20471752266132,12.4454594446349,8.11688606295397));
#10963=CARTESIAN_POINT('Ctrl Pts',(-0.21,12.4735990657963,8.11615888233178));
#10964=CARTESIAN_POINT('Ctrl Pts',(-0.21,12.5,8.11615888233178));
#10965=CARTESIAN_POINT('Ctrl Pts',(-0.21,12.5,8.11615888233178));
#10966=CARTESIAN_POINT('Ctrl Pts',(-0.21,12.5264009342037,8.11615888233178));
#10967=CARTESIAN_POINT('Ctrl Pts',(-0.20471752266132,12.5545405553651,8.11688606295397));
#10968=CARTESIAN_POINT('Ctrl Pts',(-0.183276841782292,12.6062710523005,
8.11950502964782));
#10969=CARTESIAN_POINT('Ctrl Pts',(-0.167120287247804,12.6298645608505,
8.12135816887013));
#10970=CARTESIAN_POINT('Ctrl Pts',(-0.129864750292352,12.667120097806,8.12483075953278));
#10971=CARTESIAN_POINT('Ctrl Pts',(-0.106271159541075,12.6832768008312,
8.12667690933009));
#10972=CARTESIAN_POINT('Ctrl Pts',(-0.0545403836274679,12.7047175903444,
8.12927985626981));
#10973=CARTESIAN_POINT('Ctrl Pts',(-0.0264006657112965,12.71,8.13));
#10974=CARTESIAN_POINT('Ctrl Pts',(0.0264006657112964,12.71,8.13));
#10975=CARTESIAN_POINT('Ctrl Pts',(0.0545403836274679,12.7047175903444,
8.12927985626981));
#10976=CARTESIAN_POINT('Ctrl Pts',(0.106271159541075,12.6832768008312,8.12667690933009));
#10977=CARTESIAN_POINT('Ctrl Pts',(0.129864750292352,12.667120097806,8.12483075953278));
#10978=CARTESIAN_POINT('Ctrl Pts',(0.167120287247804,12.6298645608505,8.12135816887013));
#10979=CARTESIAN_POINT('Ctrl Pts',(0.183276841782292,12.6062710523005,8.11950502964782));
#10980=CARTESIAN_POINT('Ctrl Pts',(0.20471752266132,12.5545405553651,8.11688606295397));
#10981=CARTESIAN_POINT('Ctrl Pts',(0.21,12.5264009342037,8.11615888233178));
#10982=CARTESIAN_POINT('Ctrl Pts',(0.21,12.5,8.11615888233178));
#10983=CARTESIAN_POINT('',(-0.172988438920056,12.6190588089979,7.52));
#10984=CARTESIAN_POINT('Origin',(0.,12.5,7.52));
#10985=CARTESIAN_POINT('Ctrl Pts',(0.172988438920056,12.6190588089979,7.52));
#10986=CARTESIAN_POINT('Ctrl Pts',(0.165594865311315,12.6298014223953,7.52129192197638));
#10987=CARTESIAN_POINT('Ctrl Pts',(0.157297138725606,12.6396877093727,7.52265394943905));
#10988=CARTESIAN_POINT('Ctrl Pts',(0.129892073845076,12.6670927742533,7.5267480843909));
#10989=CARTESIAN_POINT('Ctrl Pts',(0.106330167759285,12.683242056333,7.52969589327638));
#10990=CARTESIAN_POINT('Ctrl Pts',(0.0546129046324104,12.7046977939649,
7.53385029472357));
#10991=CARTESIAN_POINT('Ctrl Pts',(0.0264512308298516,12.71,7.535));
#10992=CARTESIAN_POINT('Ctrl Pts',(-0.0264512308298516,12.71,7.535));
#10993=CARTESIAN_POINT('Ctrl Pts',(-0.0546129046324104,12.7046977939649,
7.53385029472357));
#10994=CARTESIAN_POINT('Ctrl Pts',(-0.106330167759285,12.683242056333,7.52969589327638));
#10995=CARTESIAN_POINT('Ctrl Pts',(-0.129892073845076,12.6670927742533,
7.5267480843909));
#10996=CARTESIAN_POINT('Ctrl Pts',(-0.157297138725606,12.6396877093727,
7.52265394943905));
#10997=CARTESIAN_POINT('Ctrl Pts',(-0.165594865311316,12.6298014223953,
7.52129192197638));
#10998=CARTESIAN_POINT('Ctrl Pts',(-0.172988438920056,12.6190588089979,
7.52));
#10999=CARTESIAN_POINT('Origin',(0.,12.5,7.52));
#11000=CARTESIAN_POINT('',(-0.172988438920056,12.,7.52));
#11001=CARTESIAN_POINT('Origin',(0.,12.,6.53));
#11002=CARTESIAN_POINT('',(-1.005,13.,6.53));
#11003=CARTESIAN_POINT('Origin',(0.,13.,6.53));
#11004=CARTESIAN_POINT('',(-1.005,12.,6.53));
#11005=CARTESIAN_POINT('',(-1.005,12.,6.53));
#11006=CARTESIAN_POINT('Origin',(0.,12.,6.53));
#11007=CARTESIAN_POINT('Origin',(0.,12.,6.53));
#11008=CARTESIAN_POINT('',(-1.6,13.,6.53));
#11009=CARTESIAN_POINT('Origin',(0.,13.,6.53));
#11010=CARTESIAN_POINT('',(-1.6,12.,6.53));
#11011=CARTESIAN_POINT('',(-1.6,12.,6.53));
#11012=CARTESIAN_POINT('Origin',(0.,12.,6.53));
#11013=CARTESIAN_POINT('Origin',(0.,13.,6.53));
#11014=CARTESIAN_POINT('Origin',(0.,12.,6.53));
#11015=CARTESIAN_POINT('',(0.,0.,0.));
#11016=CARTESIAN_POINT('Origin',(0.,-2.4,7.52));
#11017=CARTESIAN_POINT('',(0.172988438920056,-2.51905880899792,7.52));
#11018=CARTESIAN_POINT('',(0.172988438920056,-2.28094119100208,7.52));
#11019=CARTESIAN_POINT('',(0.172988438920056,-3.6,7.52));
#11020=CARTESIAN_POINT('Origin',(0.,-2.4,7.52));
#11021=CARTESIAN_POINT('Origin',(0.,-2.4,7.52));
#11022=CARTESIAN_POINT('',(-0.172988438920056,-2.51905880899792,7.52));
#11023=CARTESIAN_POINT('Ctrl Pts',(-0.172988438920056,-2.51905880899792,
7.52));
#11024=CARTESIAN_POINT('Ctrl Pts',(-0.165594865311314,-2.52980142239529,
7.52129192197638));
#11025=CARTESIAN_POINT('Ctrl Pts',(-0.157297138725606,-2.53968770937274,
7.52265394943905));
#11026=CARTESIAN_POINT('Ctrl Pts',(-0.129892073845076,-2.56709277425327,
7.5267480843909));
#11027=CARTESIAN_POINT('Ctrl Pts',(-0.106330167759285,-2.58324205633295,
7.52969589327638));
#11028=CARTESIAN_POINT('Ctrl Pts',(-0.0546129046324105,-2.60469779396491,
7.53385029472357));
#11029=CARTESIAN_POINT('Ctrl Pts',(-0.0264512308298517,-2.61,7.535));
#11030=CARTESIAN_POINT('Ctrl Pts',(0.0264512308298516,-2.61,7.535));
#11031=CARTESIAN_POINT('Ctrl Pts',(0.0546129046324104,-2.60469779396491,
7.53385029472357));
#11032=CARTESIAN_POINT('Ctrl Pts',(0.106330167759284,-2.58324205633295,
7.52969589327638));
#11033=CARTESIAN_POINT('Ctrl Pts',(0.129892073845076,-2.56709277425327,
7.5267480843909));
#11034=CARTESIAN_POINT('Ctrl Pts',(0.157297138725606,-2.53968770937274,
7.52265394943905));
#11035=CARTESIAN_POINT('Ctrl Pts',(0.165594865311314,-2.52980142239529,
7.52129192197638));
#11036=CARTESIAN_POINT('Ctrl Pts',(0.172988438920056,-2.51905880899792,
7.52));
#11037=CARTESIAN_POINT('',(-0.21,-2.4,7.52));
#11038=CARTESIAN_POINT('Origin',(0.,-2.4,7.52));
#11039=CARTESIAN_POINT('',(-0.21,-2.4,8.11615888233178));
#11040=CARTESIAN_POINT('',(-0.21,-2.4,7.52));
#11041=CARTESIAN_POINT('',(0.21,-2.4,8.11615888233178));
#11042=CARTESIAN_POINT('Ctrl Pts',(0.21,-2.4,8.11615888233178));
#11043=CARTESIAN_POINT('Ctrl Pts',(0.21,-2.42640093420375,8.11615888233178));
#11044=CARTESIAN_POINT('Ctrl Pts',(0.20471752266132,-2.45454055536511,8.11688606295397));
#11045=CARTESIAN_POINT('Ctrl Pts',(0.183276841782292,-2.5062710523005,8.11950502964782));
#11046=CARTESIAN_POINT('Ctrl Pts',(0.167120287247804,-2.52986456085055,
8.12135816887013));
#11047=CARTESIAN_POINT('Ctrl Pts',(0.129864750292352,-2.567120097806,8.12483075953278));
#11048=CARTESIAN_POINT('Ctrl Pts',(0.106271159541076,-2.58327680083123,
8.12667690933009));
#11049=CARTESIAN_POINT('Ctrl Pts',(0.0545403836274688,-2.6047175903444,
8.12927985626981));
#11050=CARTESIAN_POINT('Ctrl Pts',(0.0264006657112965,-2.61,8.13));
#11051=CARTESIAN_POINT('Ctrl Pts',(-0.0264006657112964,-2.61,8.13));
#11052=CARTESIAN_POINT('Ctrl Pts',(-0.0545403836274688,-2.6047175903444,
8.12927985626981));
#11053=CARTESIAN_POINT('Ctrl Pts',(-0.106271159541076,-2.58327680083123,
8.12667690933009));
#11054=CARTESIAN_POINT('Ctrl Pts',(-0.129864750292352,-2.567120097806,8.12483075953278));
#11055=CARTESIAN_POINT('Ctrl Pts',(-0.167120287247804,-2.52986456085055,
8.12135816887013));
#11056=CARTESIAN_POINT('Ctrl Pts',(-0.183276841782292,-2.5062710523005,
8.11950502964782));
#11057=CARTESIAN_POINT('Ctrl Pts',(-0.20471752266132,-2.45454055536511,
8.11688606295397));
#11058=CARTESIAN_POINT('Ctrl Pts',(-0.21,-2.42640093420375,8.11615888233178));
#11059=CARTESIAN_POINT('Ctrl Pts',(-0.21,-2.4,8.11615888233178));
#11060=CARTESIAN_POINT('Ctrl Pts',(-0.21,-2.4,8.11615888233178));
#11061=CARTESIAN_POINT('Ctrl Pts',(-0.21,-2.37359906579625,8.11615888233178));
#11062=CARTESIAN_POINT('Ctrl Pts',(-0.20471752266132,-2.34545944463489,
8.11688606295397));
#11063=CARTESIAN_POINT('Ctrl Pts',(-0.183276841782292,-2.2937289476995,
8.11950502964782));
#11064=CARTESIAN_POINT('Ctrl Pts',(-0.167120287247804,-2.27013543914945,
8.12135816887013));
#11065=CARTESIAN_POINT('Ctrl Pts',(-0.129864750292352,-2.232879902194,8.12483075953278));
#11066=CARTESIAN_POINT('Ctrl Pts',(-0.106271159541076,-2.21672319916877,
8.12667690933009));
#11067=CARTESIAN_POINT('Ctrl Pts',(-0.0545403836274688,-2.1952824096556,
8.12927985626981));
#11068=CARTESIAN_POINT('Ctrl Pts',(-0.0264006657112965,-2.19,8.13));
#11069=CARTESIAN_POINT('Ctrl Pts',(0.0264006657112965,-2.19,8.13));
#11070=CARTESIAN_POINT('Ctrl Pts',(0.0545403836274689,-2.1952824096556,
8.12927985626981));
#11071=CARTESIAN_POINT('Ctrl Pts',(0.106271159541076,-2.21672319916877,
8.12667690933009));
#11072=CARTESIAN_POINT('Ctrl Pts',(0.129864750292352,-2.232879902194,8.12483075953278));
#11073=CARTESIAN_POINT('Ctrl Pts',(0.167120287247804,-2.27013543914945,
8.12135816887013));
#11074=CARTESIAN_POINT('Ctrl Pts',(0.183276841782292,-2.2937289476995,8.11950502964782));
#11075=CARTESIAN_POINT('Ctrl Pts',(0.20471752266132,-2.34545944463489,8.11688606295397));
#11076=CARTESIAN_POINT('Ctrl Pts',(0.21,-2.37359906579625,8.11615888233178));
#11077=CARTESIAN_POINT('Ctrl Pts',(0.21,-2.4,8.11615888233178));
#11078=CARTESIAN_POINT('',(-0.172988438920056,-2.28094119100208,7.52));
#11079=CARTESIAN_POINT('Origin',(0.,-2.4,7.52));
#11080=CARTESIAN_POINT('Ctrl Pts',(0.172988438920056,-2.28094119100209,
7.52));
#11081=CARTESIAN_POINT('Ctrl Pts',(0.165594865311314,-2.27019857760471,
7.52129192197638));
#11082=CARTESIAN_POINT('Ctrl Pts',(0.157297138725606,-2.26031229062726,
7.52265394943905));
#11083=CARTESIAN_POINT('Ctrl Pts',(0.129892073845076,-2.23290722574673,
7.5267480843909));
#11084=CARTESIAN_POINT('Ctrl Pts',(0.106330167759284,-2.21675794366705,
7.52969589327638));
#11085=CARTESIAN_POINT('Ctrl Pts',(0.0546129046324104,-2.19530220603509,
7.53385029472357));
#11086=CARTESIAN_POINT('Ctrl Pts',(0.0264512308298516,-2.19,7.535));
#11087=CARTESIAN_POINT('Ctrl Pts',(-0.0264512308298516,-2.19,7.535));
#11088=CARTESIAN_POINT('Ctrl Pts',(-0.0546129046324104,-2.19530220603509,
7.53385029472357));
#11089=CARTESIAN_POINT('Ctrl Pts',(-0.106330167759284,-2.21675794366705,
7.52969589327638));
#11090=CARTESIAN_POINT('Ctrl Pts',(-0.129892073845076,-2.23290722574673,
7.5267480843909));
#11091=CARTESIAN_POINT('Ctrl Pts',(-0.157297138725606,-2.26031229062726,
7.52265394943905));
#11092=CARTESIAN_POINT('Ctrl Pts',(-0.165594865311315,-2.27019857760471,
7.52129192197638));
#11093=CARTESIAN_POINT('Ctrl Pts',(-0.172988438920056,-2.28094119100208,
7.52));
#11094=CARTESIAN_POINT('Origin',(0.,-2.4,7.52));
#11095=CARTESIAN_POINT('',(-0.172988438920056,-3.6,7.52));
#11096=CARTESIAN_POINT('Origin',(0.,-2.9,6.53));
#11097=CARTESIAN_POINT('',(-1.6,-1.9,6.53));
#11098=CARTESIAN_POINT('Origin',(0.,-1.9,6.53));
#11099=CARTESIAN_POINT('',(-1.6,-2.9,6.53));
#11100=CARTESIAN_POINT('',(-1.6,-2.9,6.53));
#11101=CARTESIAN_POINT('Origin',(0.,-2.9,6.53));
#11102=CARTESIAN_POINT('Origin',(0.,-1.9,6.53));
#11103=CARTESIAN_POINT('',(-1.005,-1.9,6.53));
#11104=CARTESIAN_POINT('Origin',(0.,-1.9,6.53));
#11105=CARTESIAN_POINT('Origin',(0.,-3.6,6.53));
#11106=CARTESIAN_POINT('',(-1.005,-3.5,6.53));
#11107=CARTESIAN_POINT('Origin',(0.,-3.5,6.53));
#11108=CARTESIAN_POINT('',(-1.005,-3.6,6.53));
#11109=CARTESIAN_POINT('Origin',(4.,-3.5,6.53));
#11110=CARTESIAN_POINT('',(4.49999314610979,-3.5,6.52214602235346));
#11111=CARTESIAN_POINT('',(4.,-3.5,6.53));
#11112=CARTESIAN_POINT('',(4.49999314610979,-3.5,6.52214602235346));
#11113=CARTESIAN_POINT('',(4.49999314610979,-2.9,6.52214602235346));
#11114=CARTESIAN_POINT('',(4.49999314610979,-3.5,6.52214602235346));
#11115=CARTESIAN_POINT('',(4.,-2.9,6.53));
#11116=CARTESIAN_POINT('',(4.49999314610979,-2.9,6.52214602235346));
#11117=CARTESIAN_POINT('',(4.,-3.5,6.53));
#11118=CARTESIAN_POINT('Origin',(4.34869235694598,-3.5,7.68709756919613));
#11119=CARTESIAN_POINT('',(4.34869235694598,-3.5,7.68709756919613));
#11120=CARTESIAN_POINT('',(4.,-3.5,6.53));
#11121=CARTESIAN_POINT('',(4.34869235694598,-2.9,7.68709756919613));
#11122=CARTESIAN_POINT('',(4.,-2.9,6.53));
#11123=CARTESIAN_POINT('',(4.34869235694598,-3.5,7.68709756919613));
#11124=CARTESIAN_POINT('Origin',(3.86370330515627,-3.5,7.56527618041008));
#11125=CARTESIAN_POINT('',(3.86370330515627,-3.5,7.56527618041008));
#11126=CARTESIAN_POINT('',(4.34869235694598,-3.5,7.68709756919613));
#11127=CARTESIAN_POINT('',(3.86370330515627,-2.9,7.56527618041008));
#11128=CARTESIAN_POINT('',(4.34869235694598,-2.9,7.68709756919613));
#11129=CARTESIAN_POINT('',(3.86370330515627,-3.5,7.56527618041008));
#11130=CARTESIAN_POINT('Origin',(3.90103537021021,-3.5,8.77319482889224));
#11131=CARTESIAN_POINT('',(3.90103537021021,-3.5,8.77319482889224));
#11132=CARTESIAN_POINT('',(3.86370330515627,-3.5,7.56527618041008));
#11133=CARTESIAN_POINT('',(3.90103537021021,-2.9,8.77319482889224));
#11134=CARTESIAN_POINT('',(3.86370330515627,-2.9,7.56527618041008));
#11135=CARTESIAN_POINT('',(3.90103537021021,-3.5,8.77319482889224));
#11136=CARTESIAN_POINT('Origin',(3.46410161513775,-3.5,8.53));
#11137=CARTESIAN_POINT('',(3.46410161513775,-3.5,8.53));
#11138=CARTESIAN_POINT('',(3.90103537021021,-3.5,8.77319482889224));
#11139=CARTESIAN_POINT('',(3.46410161513775,-2.9,8.53));
#11140=CARTESIAN_POINT('',(3.90103537021021,-2.9,8.77319482889224));
#11141=CARTESIAN_POINT('',(3.46410161513775,-3.5,8.53));
#11142=CARTESIAN_POINT('Origin',(3.18752926976038,-3.5,9.70642206805406));
#11143=CARTESIAN_POINT('',(3.18752926976038,-3.5,9.70642206805406));
#11144=CARTESIAN_POINT('',(3.46410161513775,-3.5,8.53));
#11145=CARTESIAN_POINT('',(3.18752926976038,-2.9,9.70642206805406));
#11146=CARTESIAN_POINT('',(3.46410161513775,-2.9,8.53));
#11147=CARTESIAN_POINT('',(3.18752926976038,-3.5,9.70642206805406));
#11148=CARTESIAN_POINT('Origin',(2.82842712474619,-3.5,9.35842712474619));
#11149=CARTESIAN_POINT('',(2.82842712474619,-3.5,9.35842712474619));
#11150=CARTESIAN_POINT('',(3.18752926976038,-3.5,9.70642206805406));
#11151=CARTESIAN_POINT('',(2.82842712474619,-2.9,9.35842712474619));
#11152=CARTESIAN_POINT('',(3.18752926976038,-2.9,9.70642206805406));
#11153=CARTESIAN_POINT('',(2.82842712474619,-3.5,9.35842712474619));
#11154=CARTESIAN_POINT('Origin',(2.25679831721756,-3.5,10.4231813925637));
#11155=CARTESIAN_POINT('',(2.25679831721756,-3.5,10.4231813925637));
#11156=CARTESIAN_POINT('',(2.82842712474619,-3.5,9.35842712474619));
#11157=CARTESIAN_POINT('',(2.25679831721756,-2.9,10.4231813925637));
#11158=CARTESIAN_POINT('',(2.82842712474619,-2.9,9.35842712474619));
#11159=CARTESIAN_POINT('',(2.25679831721756,-3.5,10.4231813925637));
#11160=CARTESIAN_POINT('Origin',(2.,-3.5,9.99410161513775));
#11161=CARTESIAN_POINT('',(2.,-3.5,9.99410161513775));
#11162=CARTESIAN_POINT('',(2.25679831721756,-3.5,10.4231813925637));
#11163=CARTESIAN_POINT('',(2.,-2.9,9.99410161513775));
#11164=CARTESIAN_POINT('',(2.25679831721756,-2.9,10.4231813925637));
#11165=CARTESIAN_POINT('',(2.,-3.5,9.99410161513775));
#11166=CARTESIAN_POINT('Origin',(1.17227028889192,-3.5,10.8746268389565));
#11167=CARTESIAN_POINT('',(1.17227028889192,-3.5,10.8746268389565));
#11168=CARTESIAN_POINT('',(2.,-3.5,9.99410161513775));
#11169=CARTESIAN_POINT('',(1.17227028889192,-2.9,10.8746268389565));
#11170=CARTESIAN_POINT('',(2.,-2.9,9.99410161513775));
#11171=CARTESIAN_POINT('',(1.17227028889192,-3.5,10.8746268389565));
#11172=CARTESIAN_POINT('Origin',(1.03527618041008,-3.5,10.3937033051563));
#11173=CARTESIAN_POINT('',(1.03527618041008,-3.5,10.3937033051563));
#11174=CARTESIAN_POINT('',(1.17227028889192,-3.5,10.8746268389565));
#11175=CARTESIAN_POINT('',(1.03527618041008,-2.9,10.3937033051563));
#11176=CARTESIAN_POINT('',(1.17227028889192,-2.9,10.8746268389565));
#11177=CARTESIAN_POINT('',(1.03527618041008,-3.5,10.3937033051563));
#11178=CARTESIAN_POINT('Origin',(0.00785397764654228,-3.5,11.0299931461098));
#11179=CARTESIAN_POINT('',(0.00785397764654218,-3.5,11.0299931461098));
#11180=CARTESIAN_POINT('',(1.03527618041008,-3.5,10.3937033051563));
#11181=CARTESIAN_POINT('',(0.00785397764654228,-2.9,11.0299931461098));
#11182=CARTESIAN_POINT('',(1.03527618041008,-2.9,10.3937033051563));
#11183=CARTESIAN_POINT('',(0.00785397764654218,-3.5,11.0299931461098));
#11184=CARTESIAN_POINT('Origin',(2.4459601011273E-16,-3.5,10.53));
#11185=CARTESIAN_POINT('',(2.44929359829471E-16,-3.5,10.53));
#11186=CARTESIAN_POINT('',(0.00785397764654218,-3.5,11.0299931461098));
#11187=CARTESIAN_POINT('',(4.44089209850063E-16,-2.9,10.53));
#11188=CARTESIAN_POINT('',(0.00785397764654218,-2.9,11.0299931461098));
#11189=CARTESIAN_POINT('',(2.44929359829471E-16,-3.5,10.53));
#11190=CARTESIAN_POINT('Origin',(-1.15709756919613,-3.5,10.878692356946));
#11191=CARTESIAN_POINT('',(-1.15709756919613,-3.5,10.878692356946));
#11192=CARTESIAN_POINT('',(2.44929359829471E-16,-3.5,10.53));
#11193=CARTESIAN_POINT('',(-1.15709756919613,-2.9,10.878692356946));
#11194=CARTESIAN_POINT('',(2.44929359829471E-16,-2.9,10.53));
#11195=CARTESIAN_POINT('',(-1.15709756919613,-3.5,10.878692356946));
#11196=CARTESIAN_POINT('Origin',(-1.03527618041008,-3.5,10.3937033051563));
#11197=CARTESIAN_POINT('',(-1.03527618041008,-3.5,10.3937033051563));
#11198=CARTESIAN_POINT('',(-1.15709756919613,-3.5,10.878692356946));
#11199=CARTESIAN_POINT('',(-1.03527618041008,-2.9,10.3937033051563));
#11200=CARTESIAN_POINT('',(-1.15709756919613,-2.9,10.878692356946));
#11201=CARTESIAN_POINT('',(-1.03527618041008,-3.5,10.3937033051563));
#11202=CARTESIAN_POINT('Origin',(-2.24319482889224,-3.5,10.4310353702102));
#11203=CARTESIAN_POINT('',(-2.24319482889224,-3.5,10.4310353702102));
#11204=CARTESIAN_POINT('',(-1.03527618041008,-3.5,10.3937033051563));
#11205=CARTESIAN_POINT('',(-2.24319482889224,-2.9,10.4310353702102));
#11206=CARTESIAN_POINT('',(-1.03527618041008,-2.9,10.3937033051563));
#11207=CARTESIAN_POINT('',(-2.24319482889224,-3.5,10.4310353702102));
#11208=CARTESIAN_POINT('Origin',(-2.,-3.5,9.99410161513775));
#11209=CARTESIAN_POINT('',(-2.,-3.5,9.99410161513775));
#11210=CARTESIAN_POINT('',(-2.24319482889224,-3.5,10.4310353702102));
#11211=CARTESIAN_POINT('',(-2.,-2.9,9.99410161513775));
#11212=CARTESIAN_POINT('',(-2.24319482889224,-2.9,10.4310353702102));
#11213=CARTESIAN_POINT('',(-2.,-3.5,9.99410161513775));
#11214=CARTESIAN_POINT('Origin',(-3.17642206805406,-3.5,9.71752926976038));
#11215=CARTESIAN_POINT('',(-3.17642206805406,-3.5,9.71752926976038));
#11216=CARTESIAN_POINT('',(-2.,-3.5,9.99410161513775));
#11217=CARTESIAN_POINT('',(-3.17642206805406,-2.9,9.71752926976038));
#11218=CARTESIAN_POINT('',(-2.,-2.9,9.99410161513775));
#11219=CARTESIAN_POINT('',(-3.17642206805406,-3.5,9.71752926976038));
#11220=CARTESIAN_POINT('Origin',(-2.82842712474619,-3.5,9.35842712474619));
#11221=CARTESIAN_POINT('',(-2.82842712474619,-3.5,9.35842712474619));
#11222=CARTESIAN_POINT('',(-3.17642206805406,-3.5,9.71752926976038));
#11223=CARTESIAN_POINT('',(-2.82842712474619,-2.9,9.35842712474619));
#11224=CARTESIAN_POINT('',(-3.17642206805406,-2.9,9.71752926976038));
#11225=CARTESIAN_POINT('',(-2.82842712474619,-3.5,9.35842712474619));
#11226=CARTESIAN_POINT('Origin',(-3.89318139256367,-3.5,8.78679831721756));
#11227=CARTESIAN_POINT('',(-3.89318139256367,-3.5,8.78679831721756));
#11228=CARTESIAN_POINT('',(-2.82842712474619,-3.5,9.35842712474619));
#11229=CARTESIAN_POINT('',(-3.89318139256367,-2.9,8.78679831721756));
#11230=CARTESIAN_POINT('',(-2.82842712474619,-2.9,9.35842712474619));
#11231=CARTESIAN_POINT('',(-3.89318139256367,-3.5,8.78679831721756));
#11232=CARTESIAN_POINT('Origin',(-3.46410161513775,-3.5,8.53));
#11233=CARTESIAN_POINT('',(-3.46410161513775,-3.5,8.53));
#11234=CARTESIAN_POINT('',(-3.89318139256367,-3.5,8.78679831721756));
#11235=CARTESIAN_POINT('',(-3.46410161513775,-2.9,8.53));
#11236=CARTESIAN_POINT('',(-3.89318139256367,-2.9,8.78679831721756));
#11237=CARTESIAN_POINT('',(-3.46410161513775,-3.5,8.53));
#11238=CARTESIAN_POINT('Origin',(-4.34462683895651,-3.5,7.70227028889192));
#11239=CARTESIAN_POINT('',(-4.34462683895651,-3.5,7.70227028889192));
#11240=CARTESIAN_POINT('',(-3.46410161513775,-3.5,8.53));
#11241=CARTESIAN_POINT('',(-4.34462683895651,-2.9,7.70227028889192));
#11242=CARTESIAN_POINT('',(-3.46410161513775,-2.9,8.53));
#11243=CARTESIAN_POINT('',(-4.34462683895651,-3.5,7.70227028889192));
#11244=CARTESIAN_POINT('Origin',(-3.86370330515627,-3.5,7.56527618041008));
#11245=CARTESIAN_POINT('',(-3.86370330515627,-3.5,7.56527618041008));
#11246=CARTESIAN_POINT('',(-4.34462683895651,-3.5,7.70227028889192));
#11247=CARTESIAN_POINT('',(-3.86370330515627,-2.9,7.56527618041008));
#11248=CARTESIAN_POINT('',(-4.34462683895651,-2.9,7.70227028889192));
#11249=CARTESIAN_POINT('',(-3.86370330515627,-3.5,7.56527618041008));
#11250=CARTESIAN_POINT('Origin',(-4.49999314610979,-3.5,6.53785397764654));
#11251=CARTESIAN_POINT('',(-4.49999314610979,-3.5,6.53785397764654));
#11252=CARTESIAN_POINT('',(-3.86370330515627,-3.5,7.56527618041008));
#11253=CARTESIAN_POINT('',(-4.49999314610979,-2.9,6.53785397764654));
#11254=CARTESIAN_POINT('',(-3.86370330515627,-2.9,7.56527618041008));
#11255=CARTESIAN_POINT('',(-4.49999314610979,-3.5,6.53785397764654));
#11256=CARTESIAN_POINT('Origin',(-4.,-3.5,6.53));
#11257=CARTESIAN_POINT('',(-4.,-3.5,6.53));
#11258=CARTESIAN_POINT('',(-4.49999314610979,-3.5,6.53785397764654));
#11259=CARTESIAN_POINT('',(-4.,-2.9,6.53));
#11260=CARTESIAN_POINT('',(-4.49999314610979,-2.9,6.53785397764654));
#11261=CARTESIAN_POINT('',(-4.,-3.5,6.53));
#11262=CARTESIAN_POINT('Origin',(-4.34869235694598,-3.5,5.37290243080387));
#11263=CARTESIAN_POINT('',(-4.34869235694598,-3.5,5.37290243080387));
#11264=CARTESIAN_POINT('',(-4.,-3.5,6.53));
#11265=CARTESIAN_POINT('',(-4.34869235694598,-2.9,5.37290243080387));
#11266=CARTESIAN_POINT('',(-4.,-2.9,6.53));
#11267=CARTESIAN_POINT('',(-4.34869235694598,-3.5,5.37290243080387));
#11268=CARTESIAN_POINT('Origin',(-3.86370330515627,-3.5,5.49472381958992));
#11269=CARTESIAN_POINT('',(-3.86370330515627,-3.5,5.49472381958992));
#11270=CARTESIAN_POINT('',(-4.34869235694598,-3.5,5.37290243080387));
#11271=CARTESIAN_POINT('',(-3.86370330515627,-2.9,5.49472381958992));
#11272=CARTESIAN_POINT('',(-4.34869235694598,-2.9,5.37290243080387));
#11273=CARTESIAN_POINT('',(-3.86370330515627,-3.5,5.49472381958992));
#11274=CARTESIAN_POINT('Origin',(-3.90103537021021,-3.5,4.28680517110776));
#11275=CARTESIAN_POINT('',(-3.90103537021021,-3.5,4.28680517110776));
#11276=CARTESIAN_POINT('',(-3.86370330515627,-3.5,5.49472381958992));
#11277=CARTESIAN_POINT('',(-3.90103537021021,-2.9,4.28680517110776));
#11278=CARTESIAN_POINT('',(-3.86370330515627,-2.9,5.49472381958992));
#11279=CARTESIAN_POINT('',(-3.90103537021021,-3.5,4.28680517110776));
#11280=CARTESIAN_POINT('Origin',(-3.46410161513775,-3.5,4.53));
#11281=CARTESIAN_POINT('',(-3.46410161513775,-3.5,4.53));
#11282=CARTESIAN_POINT('',(-3.90103537021021,-3.5,4.28680517110776));
#11283=CARTESIAN_POINT('',(-3.46410161513775,-2.9,4.53));
#11284=CARTESIAN_POINT('',(-3.90103537021021,-2.9,4.28680517110776));
#11285=CARTESIAN_POINT('',(-3.46410161513775,-3.5,4.53));
#11286=CARTESIAN_POINT('Origin',(-3.18752926976038,-3.5,3.35357793194594));
#11287=CARTESIAN_POINT('',(-3.18752926976038,-3.5,3.35357793194594));
#11288=CARTESIAN_POINT('',(-3.46410161513775,-3.5,4.53));
#11289=CARTESIAN_POINT('',(-3.18752926976038,-2.9,3.35357793194594));
#11290=CARTESIAN_POINT('',(-3.46410161513775,-2.9,4.53));
#11291=CARTESIAN_POINT('',(-3.18752926976038,-3.5,3.35357793194594));
#11292=CARTESIAN_POINT('Origin',(-2.82842712474619,-3.5,3.70157287525381));
#11293=CARTESIAN_POINT('',(-2.82842712474619,-3.5,3.70157287525381));
#11294=CARTESIAN_POINT('',(-3.18752926976038,-3.5,3.35357793194594));
#11295=CARTESIAN_POINT('',(-2.82842712474619,-2.9,3.70157287525381));
#11296=CARTESIAN_POINT('',(-3.18752926976038,-2.9,3.35357793194594));
#11297=CARTESIAN_POINT('',(-2.82842712474619,-3.5,3.70157287525381));
#11298=CARTESIAN_POINT('Origin',(-2.25679831721756,-3.5,2.63681860743633));
#11299=CARTESIAN_POINT('',(-2.25679831721756,-3.5,2.63681860743633));
#11300=CARTESIAN_POINT('',(-2.82842712474619,-3.5,3.70157287525381));
#11301=CARTESIAN_POINT('',(-2.25679831721756,-2.9,2.63681860743633));
#11302=CARTESIAN_POINT('',(-2.82842712474619,-2.9,3.70157287525381));
#11303=CARTESIAN_POINT('',(-2.25679831721756,-3.5,2.63681860743633));
#11304=CARTESIAN_POINT('Origin',(-2.,-3.5,3.06589838486225));
#11305=CARTESIAN_POINT('',(-2.,-3.5,3.06589838486225));
#11306=CARTESIAN_POINT('',(-2.25679831721756,-3.5,2.63681860743633));
#11307=CARTESIAN_POINT('',(-2.,-2.9,3.06589838486225));
#11308=CARTESIAN_POINT('',(-2.25679831721756,-2.9,2.63681860743633));
#11309=CARTESIAN_POINT('',(-2.,-3.5,3.06589838486225));
#11310=CARTESIAN_POINT('Origin',(-1.17227028889192,-3.5,2.18537316104349));
#11311=CARTESIAN_POINT('',(-1.17227028889192,-3.5,2.18537316104349));
#11312=CARTESIAN_POINT('',(-2.,-3.5,3.06589838486225));
#11313=CARTESIAN_POINT('',(-1.17227028889192,-2.9,2.18537316104349));
#11314=CARTESIAN_POINT('',(-2.,-2.9,3.06589838486225));
#11315=CARTESIAN_POINT('',(-1.17227028889192,-3.5,2.18537316104349));
#11316=CARTESIAN_POINT('Origin',(-1.03527618041008,-3.5,2.66629669484373));
#11317=CARTESIAN_POINT('',(-1.03527618041008,-3.5,2.66629669484373));
#11318=CARTESIAN_POINT('',(-1.17227028889192,-3.5,2.18537316104349));
#11319=CARTESIAN_POINT('',(-1.03527618041008,-2.9,2.66629669484373));
#11320=CARTESIAN_POINT('',(-1.17227028889192,-2.9,2.18537316104349));
#11321=CARTESIAN_POINT('',(-1.03527618041008,-3.5,2.66629669484373));
#11322=CARTESIAN_POINT('Origin',(-0.00785397764654272,-3.5,2.03000685389021));
#11323=CARTESIAN_POINT('',(-0.00785397764654273,-3.5,2.03000685389021));
#11324=CARTESIAN_POINT('',(-1.03527618041008,-3.5,2.66629669484373));
#11325=CARTESIAN_POINT('',(-0.00785397764654272,-2.9,2.03000685389021));
#11326=CARTESIAN_POINT('',(-1.03527618041008,-2.9,2.66629669484373));
#11327=CARTESIAN_POINT('',(-0.00785397764654273,-3.5,2.03000685389021));
#11328=CARTESIAN_POINT('Origin',(-7.35522753814166E-16,-3.5,2.53));
#11329=CARTESIAN_POINT('',(-7.34788079488412E-16,-3.5,2.53));
#11330=CARTESIAN_POINT('',(-0.00785397764654273,-3.5,2.03000685389021));
#11331=CARTESIAN_POINT('',(-8.88178419700125E-16,-2.9,2.53));
#11332=CARTESIAN_POINT('',(-0.00785397764654273,-2.9,2.03000685389021));
#11333=CARTESIAN_POINT('',(-7.34788079488412E-16,-3.5,2.53));
#11334=CARTESIAN_POINT('Origin',(1.15709756919613,-3.5,2.18130764305402));
#11335=CARTESIAN_POINT('',(1.15709756919613,-3.5,2.18130764305402));
#11336=CARTESIAN_POINT('',(-7.34788079488412E-16,-3.5,2.53));
#11337=CARTESIAN_POINT('',(1.15709756919613,-2.9,2.18130764305402));
#11338=CARTESIAN_POINT('',(-7.34788079488412E-16,-2.9,2.53));
#11339=CARTESIAN_POINT('',(1.15709756919613,-3.5,2.18130764305402));
#11340=CARTESIAN_POINT('Origin',(1.03527618041008,-3.5,2.66629669484373));
#11341=CARTESIAN_POINT('',(1.03527618041008,-3.5,2.66629669484373));
#11342=CARTESIAN_POINT('',(1.15709756919613,-3.5,2.18130764305402));
#11343=CARTESIAN_POINT('',(1.03527618041008,-2.9,2.66629669484373));
#11344=CARTESIAN_POINT('',(1.15709756919613,-2.9,2.18130764305402));
#11345=CARTESIAN_POINT('',(1.03527618041008,-3.5,2.66629669484373));
#11346=CARTESIAN_POINT('Origin',(2.24319482889223,-3.5,2.62896462978979));
#11347=CARTESIAN_POINT('',(2.24319482889223,-3.5,2.62896462978979));
#11348=CARTESIAN_POINT('',(1.03527618041008,-3.5,2.66629669484373));
#11349=CARTESIAN_POINT('',(2.24319482889223,-2.9,2.62896462978979));
#11350=CARTESIAN_POINT('',(1.03527618041008,-2.9,2.66629669484373));
#11351=CARTESIAN_POINT('',(2.24319482889223,-3.5,2.62896462978979));
#11352=CARTESIAN_POINT('Origin',(2.,-3.5,3.06589838486225));
#11353=CARTESIAN_POINT('',(2.,-3.5,3.06589838486225));
#11354=CARTESIAN_POINT('',(2.24319482889223,-3.5,2.62896462978979));
#11355=CARTESIAN_POINT('',(2.,-2.9,3.06589838486225));
#11356=CARTESIAN_POINT('',(2.24319482889223,-2.9,2.62896462978979));
#11357=CARTESIAN_POINT('',(2.,-3.5,3.06589838486225));
#11358=CARTESIAN_POINT('Origin',(3.17642206805406,-3.5,3.34247073023962));
#11359=CARTESIAN_POINT('',(3.17642206805406,-3.5,3.34247073023962));
#11360=CARTESIAN_POINT('',(2.,-3.5,3.06589838486225));
#11361=CARTESIAN_POINT('',(3.17642206805406,-2.9,3.34247073023962));
#11362=CARTESIAN_POINT('',(2.,-2.9,3.06589838486225));
#11363=CARTESIAN_POINT('',(3.17642206805406,-3.5,3.34247073023962));
#11364=CARTESIAN_POINT('Origin',(2.82842712474619,-3.5,3.70157287525381));
#11365=CARTESIAN_POINT('',(2.82842712474619,-3.5,3.70157287525381));
#11366=CARTESIAN_POINT('',(3.17642206805406,-3.5,3.34247073023962));
#11367=CARTESIAN_POINT('',(2.82842712474619,-2.9,3.70157287525381));
#11368=CARTESIAN_POINT('',(3.17642206805406,-2.9,3.34247073023962));
#11369=CARTESIAN_POINT('',(2.82842712474619,-3.5,3.70157287525381));
#11370=CARTESIAN_POINT('Origin',(3.89318139256367,-3.5,4.27320168278244));
#11371=CARTESIAN_POINT('',(3.89318139256367,-3.5,4.27320168278244));
#11372=CARTESIAN_POINT('',(2.82842712474619,-3.5,3.70157287525381));
#11373=CARTESIAN_POINT('',(3.89318139256367,-2.9,4.27320168278244));
#11374=CARTESIAN_POINT('',(2.82842712474619,-2.9,3.70157287525381));
#11375=CARTESIAN_POINT('',(3.89318139256367,-3.5,4.27320168278244));
#11376=CARTESIAN_POINT('Origin',(3.46410161513775,-3.5,4.53));
#11377=CARTESIAN_POINT('',(3.46410161513775,-3.5,4.53));
#11378=CARTESIAN_POINT('',(3.89318139256367,-3.5,4.27320168278244));
#11379=CARTESIAN_POINT('',(3.46410161513775,-2.9,4.53));
#11380=CARTESIAN_POINT('',(3.89318139256367,-2.9,4.27320168278244));
#11381=CARTESIAN_POINT('',(3.46410161513775,-3.5,4.53));
#11382=CARTESIAN_POINT('Origin',(4.34462683895651,-3.5,5.35772971110808));
#11383=CARTESIAN_POINT('',(4.34462683895651,-3.5,5.35772971110808));
#11384=CARTESIAN_POINT('',(3.46410161513775,-3.5,4.53));
#11385=CARTESIAN_POINT('',(4.34462683895651,-2.9,5.35772971110808));
#11386=CARTESIAN_POINT('',(3.46410161513775,-2.9,4.53));
#11387=CARTESIAN_POINT('',(4.34462683895651,-3.5,5.35772971110808));
#11388=CARTESIAN_POINT('Origin',(3.86370330515627,-3.5,5.49472381958992));
#11389=CARTESIAN_POINT('',(3.86370330515627,-3.5,5.49472381958992));
#11390=CARTESIAN_POINT('',(4.34462683895651,-3.5,5.35772971110808));
#11391=CARTESIAN_POINT('',(3.86370330515627,-2.9,5.49472381958992));
#11392=CARTESIAN_POINT('',(4.34462683895651,-2.9,5.35772971110808));
#11393=CARTESIAN_POINT('',(3.86370330515627,-3.5,5.49472381958992));
#11394=CARTESIAN_POINT('Origin',(4.49999314610979,-3.5,6.52214602235346));
#11395=CARTESIAN_POINT('',(3.86370330515627,-3.5,5.49472381958992));
#11396=CARTESIAN_POINT('',(3.86370330515627,-2.9,5.49472381958992));
#11397=CARTESIAN_POINT('Origin',(0.,-2.9,6.53));
#11398=CARTESIAN_POINT('Origin',(0.,-3.5,6.53));
#11399=CARTESIAN_POINT('',(0.,0.,0.));
#11400=CARTESIAN_POINT('Origin',(0.,-6.6,10.03));
#11401=CARTESIAN_POINT('',(-0.275,-6.5,10.03));
#11402=CARTESIAN_POINT('Origin',(0.,-6.5,10.03));
#11403=CARTESIAN_POINT('',(-0.275,-5.7,10.03));
#11404=CARTESIAN_POINT('',(-0.275,-6.6,10.03));
#11405=CARTESIAN_POINT('Origin',(0.,-5.7,10.03));
#11406=CARTESIAN_POINT('Origin',(0.,-6.,7.52));
#11407=CARTESIAN_POINT('',(0.172988438920056,-6.11905880899792,7.52));
#11408=CARTESIAN_POINT('',(0.172988438920056,-5.88094119100209,7.52));
#11409=CARTESIAN_POINT('',(0.172988438920056,-6.5,7.52));
#11410=CARTESIAN_POINT('Origin',(0.,-6.,7.52));
#11411=CARTESIAN_POINT('Origin',(0.,-6.,7.52));
#11412=CARTESIAN_POINT('',(-0.172988438920056,-6.11905880899792,7.52));
#11413=CARTESIAN_POINT('Ctrl Pts',(-0.172988438920056,-6.11905880899792,
7.52));
#11414=CARTESIAN_POINT('Ctrl Pts',(-0.165594865311313,-6.12980142239529,
7.52129192197638));
#11415=CARTESIAN_POINT('Ctrl Pts',(-0.157297138725606,-6.13968770937274,
7.52265394943905));
#11416=CARTESIAN_POINT('Ctrl Pts',(-0.129892073845076,-6.16709277425327,
7.5267480843909));
#11417=CARTESIAN_POINT('Ctrl Pts',(-0.106330167759284,-6.18324205633295,
7.52969589327638));
#11418=CARTESIAN_POINT('Ctrl Pts',(-0.05461290463241,-6.20469779396491,
7.53385029472357));
#11419=CARTESIAN_POINT('Ctrl Pts',(-0.0264512308298516,-6.21,7.535));
#11420=CARTESIAN_POINT('Ctrl Pts',(0.0264512308298515,-6.21,7.535));
#11421=CARTESIAN_POINT('Ctrl Pts',(0.0546129046324099,-6.20469779396491,
7.53385029472357));
#11422=CARTESIAN_POINT('Ctrl Pts',(0.106330167759284,-6.18324205633295,
7.52969589327638));
#11423=CARTESIAN_POINT('Ctrl Pts',(0.129892073845076,-6.16709277425327,
7.5267480843909));
#11424=CARTESIAN_POINT('Ctrl Pts',(0.157297138725606,-6.13968770937274,
7.52265394943905));
#11425=CARTESIAN_POINT('Ctrl Pts',(0.165594865311314,-6.12980142239529,
7.52129192197638));
#11426=CARTESIAN_POINT('Ctrl Pts',(0.172988438920056,-6.11905880899792,
7.52));
#11427=CARTESIAN_POINT('',(-0.21,-6.,7.52));
#11428=CARTESIAN_POINT('Origin',(0.,-6.,7.52));
#11429=CARTESIAN_POINT('',(-0.21,-6.,8.32));
#11430=CARTESIAN_POINT('',(-0.21,-6.,7.52));
#11431=CARTESIAN_POINT('Origin',(0.,-6.,8.32));
#11432=CARTESIAN_POINT('',(-0.172988438920056,-5.88094119100209,7.52));
#11433=CARTESIAN_POINT('Origin',(0.,-6.,7.52));
#11434=CARTESIAN_POINT('Ctrl Pts',(0.172988438920056,-5.88094119100209,
7.52));
#11435=CARTESIAN_POINT('Ctrl Pts',(0.165594865311314,-5.87019857760471,
7.52129192197638));
#11436=CARTESIAN_POINT('Ctrl Pts',(0.157297138725606,-5.86031229062726,
7.52265394943905));
#11437=CARTESIAN_POINT('Ctrl Pts',(0.129892073845076,-5.83290722574673,
7.5267480843909));
#11438=CARTESIAN_POINT('Ctrl Pts',(0.106330167759284,-5.81675794366705,
7.52969589327638));
#11439=CARTESIAN_POINT('Ctrl Pts',(0.05461290463241,-5.79530220603509,7.53385029472357));
#11440=CARTESIAN_POINT('Ctrl Pts',(0.0264512308298516,-5.79,7.535));
#11441=CARTESIAN_POINT('Ctrl Pts',(-0.0264512308298515,-5.79,7.535));
#11442=CARTESIAN_POINT('Ctrl Pts',(-0.0546129046324109,-5.79530220603509,
7.53385029472357));
#11443=CARTESIAN_POINT('Ctrl Pts',(-0.106330167759285,-5.81675794366705,
7.52969589327638));
#11444=CARTESIAN_POINT('Ctrl Pts',(-0.129892073845076,-5.83290722574673,
7.5267480843909));
#11445=CARTESIAN_POINT('Ctrl Pts',(-0.157297138725607,-5.86031229062726,
7.52265394943905));
#11446=CARTESIAN_POINT('Ctrl Pts',(-0.165594865311314,-5.87019857760471,
7.52129192197638));
#11447=CARTESIAN_POINT('Ctrl Pts',(-0.172988438920057,-5.88094119100209,
7.52));
#11448=CARTESIAN_POINT('Origin',(0.,-6.,8.32));
#11449=CARTESIAN_POINT('Origin',(0.,-6.,7.52));
#11450=CARTESIAN_POINT('',(-0.172988438920056,-6.5,7.52));
#11451=CARTESIAN_POINT('Origin',(0.,-6.5,6.53));
#11452=CARTESIAN_POINT('',(0.6,-6.5,8.01323969741913));
#11453=CARTESIAN_POINT('',(-1.6,-6.5,6.53));
#11454=CARTESIAN_POINT('Origin',(0.,-6.5,6.53));
#11455=CARTESIAN_POINT('',(0.6,-6.5,10.53));
#11456=CARTESIAN_POINT('',(0.6,-6.5,6.53));
#11457=CARTESIAN_POINT('',(-0.6,-6.5,10.53));
#11458=CARTESIAN_POINT('',(0.6,-6.5,10.53));
#11459=CARTESIAN_POINT('',(-0.6,-6.5,8.01323969741913));
#11460=CARTESIAN_POINT('',(-0.6,-6.5,10.53));
#11461=CARTESIAN_POINT('Origin',(0.,-6.5,6.53));
#11462=CARTESIAN_POINT('',(-1.005,-6.5,6.53));
#11463=CARTESIAN_POINT('Origin',(0.,-6.5,6.53));
#11464=CARTESIAN_POINT('Origin',(-0.6,-6.5,6.53));
#11465=CARTESIAN_POINT('',(-0.6,-5.7,8.01323969741913));
#11466=CARTESIAN_POINT('',(-0.6,-6.5,8.01323969741913));
#11467=CARTESIAN_POINT('',(-0.6,-5.7,10.53));
#11468=CARTESIAN_POINT('',(-0.6,-6.5,10.53));
#11469=CARTESIAN_POINT('',(-0.6,-5.7,10.53));
#11470=CARTESIAN_POINT('Origin',(0.,-5.7,8.53));
#11471=CARTESIAN_POINT('',(0.6,-5.7,8.01323969741913));
#11472=CARTESIAN_POINT('Origin',(0.,-5.7,6.53));
#11473=CARTESIAN_POINT('',(0.6,-5.7,10.53));
#11474=CARTESIAN_POINT('',(0.6,-5.7,10.53));
#11475=CARTESIAN_POINT('',(0.6,-5.7,6.53));
#11476=CARTESIAN_POINT('Origin',(0.6,-6.5,10.53));
#11477=CARTESIAN_POINT('',(0.6,-6.5,8.01323969741913));
#11478=CARTESIAN_POINT('',(0.6,-6.5,10.53));
#11479=CARTESIAN_POINT('Origin',(-0.6,-6.5,10.53));
#11480=CARTESIAN_POINT('Origin',(0.,-6.5,6.53));
#11481=CARTESIAN_POINT('',(-1.6,-5.5,6.53));
#11482=CARTESIAN_POINT('Origin',(0.,-5.5,6.53));
#11483=CARTESIAN_POINT('',(-1.6,-6.5,6.53));
#11484=CARTESIAN_POINT('Origin',(0.,-6.5,6.53));
#11485=CARTESIAN_POINT('',(-1.005,-5.5,6.53));
#11486=CARTESIAN_POINT('Origin',(0.,-5.5,6.53));
#11487=CARTESIAN_POINT('',(-1.005,-6.5,6.53));
#11488=CARTESIAN_POINT('Origin',(0.,-5.5,6.53));
#11489=CARTESIAN_POINT('',(0.,0.,0.));
#11490=CARTESIAN_POINT('Origin',(0.,-7.7,10.03));
#11491=CARTESIAN_POINT('',(-0.21,-7.7,10.03));
#11492=CARTESIAN_POINT('Origin',(0.,-7.7,10.03));
#11493=CARTESIAN_POINT('',(-0.21,-6.5,10.03));
#11494=CARTESIAN_POINT('',(-0.21,-7.7,10.03));
#11495=CARTESIAN_POINT('Origin',(0.,-6.5,10.03));
#11496=CARTESIAN_POINT('Origin',(0.,-7.7,10.03));
#11497=CARTESIAN_POINT('Origin',(0.,-9.5,10.03));
#11498=CARTESIAN_POINT('',(-0.7,-6.5,10.03));
#11499=CARTESIAN_POINT('Origin',(0.,-6.5,10.03));
#11500=CARTESIAN_POINT('',(-0.7,-9.5,10.03));
#11501=CARTESIAN_POINT('',(-0.7,-9.5,10.03));
#11502=CARTESIAN_POINT('Origin',(0.,-9.5,10.03));
#11503=CARTESIAN_POINT('Origin',(0.,-6.5,10.03));
#11504=CARTESIAN_POINT('Origin',(0.,-9.5,10.03));
#11505=CARTESIAN_POINT('',(0.,0.,0.));
#11506=CARTESIAN_POINT('Origin',(0.0721687836487032,0.,-0.125));
#11507=CARTESIAN_POINT('',(0.0721687836487032,0.,-0.125));
#11508=CARTESIAN_POINT('',(0.144337567297406,0.,0.));
#11509=CARTESIAN_POINT('',(0.117710979560879,0.,-0.0461186027918559));
#11510=CARTESIAN_POINT('',(0.0721687836487032,-0.25,-0.125));
#11511=CARTESIAN_POINT('',(0.0721687836487032,0.,-0.125));
#11512=CARTESIAN_POINT('',(0.144337567297406,-0.25,0.));
#11513=CARTESIAN_POINT('',(0.144337567297406,-0.25,0.));
#11514=CARTESIAN_POINT('',(0.144337567297406,0.,0.));
#11515=CARTESIAN_POINT('Origin',(-0.0721687836487032,0.,-0.125));
#11516=CARTESIAN_POINT('',(-0.0721687836487032,0.,-0.125));
#11517=CARTESIAN_POINT('',(0.0739156081756484,0.,-0.125));
#11518=CARTESIAN_POINT('',(-0.0721687836487032,-0.25,-0.125));
#11519=CARTESIAN_POINT('',(-0.0721687836487032,0.,-0.125));
#11520=CARTESIAN_POINT('',(0.0721687836487032,-0.25,-0.125));
#11521=CARTESIAN_POINT('Origin',(-0.144337567297406,0.,-4.16333634234434E-17));
#11522=CARTESIAN_POINT('',(-0.144337567297406,0.,-1.76762539787485E-17));
#11523=CARTESIAN_POINT('',(-0.0987953713852306,0.,-0.0788813972081442));
#11524=CARTESIAN_POINT('',(-0.144337567297406,-0.25,-2.77555756156289E-17));
#11525=CARTESIAN_POINT('',(-0.144337567297406,0.,-1.76762539787485E-17));
#11526=CARTESIAN_POINT('',(-0.0721687836487032,-0.25,-0.125));
#11527=CARTESIAN_POINT('Origin',(-0.0721687836487033,0.,0.125));
#11528=CARTESIAN_POINT('',(-0.0721687836487033,0.,0.125));
#11529=CARTESIAN_POINT('',(-0.0627109795608791,0.,0.141381397208144));
#11530=CARTESIAN_POINT('',(-0.0721687836487033,-0.25,0.125));
#11531=CARTESIAN_POINT('',(-0.0721687836487033,0.,0.125));
#11532=CARTESIAN_POINT('',(-0.144337567297406,-0.25,-1.76762539787485E-17));
#11533=CARTESIAN_POINT('Origin',(0.0721687836487032,0.,0.125));
#11534=CARTESIAN_POINT('',(0.0721687836487032,0.,0.125));
#11535=CARTESIAN_POINT('',(0.146084391824352,0.,0.125));
#11536=CARTESIAN_POINT('',(0.0721687836487032,-0.25,0.125));
#11537=CARTESIAN_POINT('',(0.0721687836487032,0.,0.125));
#11538=CARTESIAN_POINT('',(-0.0721687836487033,-0.25,0.125));
#11539=CARTESIAN_POINT('Origin',(0.144337567297406,0.,0.));
#11540=CARTESIAN_POINT('',(0.153795371385231,0.,-0.0163813972081441));
#11541=CARTESIAN_POINT('',(0.0721687836487032,-0.25,0.125));
#11542=CARTESIAN_POINT('Origin',(0.,-0.25,0.));
#11543=CARTESIAN_POINT('Origin',(0.22,0.,0.));
#11544=CARTESIAN_POINT('',(-0.22,-8.67361737988404E-18,-2.69422295812418E-17));
#11545=CARTESIAN_POINT('Origin',(0.,0.,0.));
#11546=CARTESIAN_POINT('Origin',(0.,-0.015,0.));
#11547=CARTESIAN_POINT('',(-0.24505,-0.02505,-3.00099698131059E-17));
#11548=CARTESIAN_POINT('Origin',(0.,-0.02505,0.));
#11549=CARTESIAN_POINT('',(-0.235,-0.015,-2.87791997799628E-17));
#11550=CARTESIAN_POINT('Origin',(0.,-0.3775,0.));
#11551=CARTESIAN_POINT('',(-0.24505,-0.72995,3.00099698131059E-17));
#11552=CARTESIAN_POINT('Origin',(0.,-0.72995,0.));
#11553=CARTESIAN_POINT('',(-0.24505,-0.3775,-3.00099698131059E-17));
#11554=CARTESIAN_POINT('Origin',(0.,-0.7625,0.));
#11555=CARTESIAN_POINT('',(-0.175,-0.8,-2.14313189850787E-17));
#11556=CARTESIAN_POINT('Origin',(0.,-0.8,0.));
#11557=CARTESIAN_POINT('',(-0.2125,-0.7625,-2.60237444818813E-17));
#11558=CARTESIAN_POINT('Origin',(0.,-0.8,0.));
#11559=CARTESIAN_POINT('',(0.,0.,0.));
#11560=CARTESIAN_POINT('Origin',(0.375,0.5,0.));
#11561=CARTESIAN_POINT('',(-0.375,0.5,-4.59242549680257E-17));
#11562=CARTESIAN_POINT('Origin',(0.,0.5,0.));
#11563=CARTESIAN_POINT('Origin',(0.,0.475,0.));
#11564=CARTESIAN_POINT('',(-0.425,0.45,-5.20474889637625E-17));
#11565=CARTESIAN_POINT('Origin',(0.,0.45,0.));
#11566=CARTESIAN_POINT('',(-0.4,0.475,-4.89858719658941E-17));
#11567=CARTESIAN_POINT('Origin',(0.,0.24,0.));
#11568=CARTESIAN_POINT('',(-0.425,0.0299999999999998,-5.20474889637625E-17));
#11569=CARTESIAN_POINT('Origin',(0.,0.0299999999999998,0.));
#11570=CARTESIAN_POINT('',(-0.425,0.24,-5.20474889637625E-17));
#11571=CARTESIAN_POINT('Origin',(0.,0.0150000000000001,0.));
#11572=CARTESIAN_POINT('',(-0.395,4.85722573273506E-17,-4.83735485663204E-17));
#11573=CARTESIAN_POINT('Origin',(0.,0.,0.));
#11574=CARTESIAN_POINT('',(-0.41,0.0150000000000001,-5.02105187650415E-17));
#11575=CARTESIAN_POINT('Origin',(0.27,0.,0.));
#11576=CARTESIAN_POINT('',(-0.27,0.,-3.30654635769785E-17));
#11577=CARTESIAN_POINT('Origin',(0.,0.,0.));
#11578=CARTESIAN_POINT('Origin',(0.,-0.02,0.));
#11579=CARTESIAN_POINT('',(-0.24505,-0.0498999999999999,3.00099698131059E-17));
#11580=CARTESIAN_POINT('Origin',(0.,-0.0498999999999999,0.));
#11581=CARTESIAN_POINT('',(-0.26,-0.02,-3.18408167778312E-17));
#11582=CARTESIAN_POINT('Origin',(0.,-0.995,0.));
#11583=CARTESIAN_POINT('',(-0.24505,-1.95495,3.00099698131059E-17));
#11584=CARTESIAN_POINT('Origin',(0.,-1.95495,0.));
#11585=CARTESIAN_POINT('',(-0.24505,-0.995,-3.00099698131059E-17));
#11586=CARTESIAN_POINT('Origin',(0.,-1.975,0.));
#11587=CARTESIAN_POINT('',(-0.2,-2.,-2.44929359829471E-17));
#11588=CARTESIAN_POINT('Origin',(0.,-2.,0.));
#11589=CARTESIAN_POINT('',(-0.225,-1.975,-2.75545529808154E-17));
#11590=CARTESIAN_POINT('Origin',(0.,-2.,0.));
#11591=CARTESIAN_POINT('Origin',(0.115470053837925,-0.5,-0.2));
#11592=CARTESIAN_POINT('',(0.23094010767585,-0.5,0.));
#11593=CARTESIAN_POINT('',(0.115470053837925,-0.5,-0.2));
#11594=CARTESIAN_POINT('',(0.23094010767585,-0.5,0.));
#11595=CARTESIAN_POINT('',(0.115470053837925,-0.8,-0.2));
#11596=CARTESIAN_POINT('',(0.115470053837925,-0.5,-0.2));
#11597=CARTESIAN_POINT('',(0.23094010767585,-0.8,0.));
#11598=CARTESIAN_POINT('',(0.23094010767585,-0.8,0.));
#11599=CARTESIAN_POINT('',(0.23094010767585,-0.5,0.));
#11600=CARTESIAN_POINT('Origin',(-0.115470053837925,-0.5,-0.2));
#11601=CARTESIAN_POINT('',(-0.115470053837925,-0.5,-0.2));
#11602=CARTESIAN_POINT('',(0.115470053837925,-0.5,-0.2));
#11603=CARTESIAN_POINT('',(-0.115470053837925,-0.8,-0.2));
#11604=CARTESIAN_POINT('',(-0.115470053837925,-0.5,-0.2));
#11605=CARTESIAN_POINT('',(0.115470053837925,-0.8,-0.2));
#11606=CARTESIAN_POINT('Origin',(-0.23094010767585,-0.5,-2.77555756156289E-17));
#11607=CARTESIAN_POINT('',(-0.23094010767585,-0.5,-2.82820063659975E-17));
#11608=CARTESIAN_POINT('',(-0.115470053837925,-0.5,-0.2));
#11609=CARTESIAN_POINT('',(-0.23094010767585,-0.8,-2.77555756156289E-17));
#11610=CARTESIAN_POINT('',(-0.23094010767585,-0.5,-2.82820063659975E-17));
#11611=CARTESIAN_POINT('',(-0.115470053837925,-0.8,-0.2));
#11612=CARTESIAN_POINT('Origin',(-0.115470053837925,-0.5,0.2));
#11613=CARTESIAN_POINT('',(-0.115470053837925,-0.5,0.2));
#11614=CARTESIAN_POINT('',(-0.23094010767585,-0.5,-2.82820063659975E-17));
#11615=CARTESIAN_POINT('',(-0.115470053837925,-0.8,0.2));
#11616=CARTESIAN_POINT('',(-0.115470053837925,-0.5,0.2));
#11617=CARTESIAN_POINT('',(-0.23094010767585,-0.8,-2.82820063659975E-17));
#11618=CARTESIAN_POINT('Origin',(0.115470053837925,-0.5,0.2));
#11619=CARTESIAN_POINT('',(0.115470053837925,-0.5,0.2));
#11620=CARTESIAN_POINT('',(-0.115470053837925,-0.5,0.2));
#11621=CARTESIAN_POINT('',(0.115470053837925,-0.8,0.2));
#11622=CARTESIAN_POINT('',(0.115470053837925,-0.5,0.2));
#11623=CARTESIAN_POINT('',(-0.115470053837925,-0.8,0.2));
#11624=CARTESIAN_POINT('Origin',(0.23094010767585,-0.5,0.));
#11625=CARTESIAN_POINT('',(0.115470053837925,-0.5,0.2));
#11626=CARTESIAN_POINT('',(0.115470053837925,-0.8,0.2));
#11627=CARTESIAN_POINT('Origin',(0.,-0.5,0.));
#11628=CARTESIAN_POINT('Origin',(0.,-0.8,0.));
#11629=CARTESIAN_POINT('',(0.,0.,0.));
#11630=CARTESIAN_POINT('',(0.,0.,0.));
#11631=CARTESIAN_POINT('',(0.,0.,0.));
#11632=CARTESIAN_POINT('',(0.,0.,0.));
#11633=CARTESIAN_POINT('',(0.,0.,0.));
#11634=CARTESIAN_POINT('',(0.,0.,0.));
#11635=CARTESIAN_POINT('',(0.,0.,0.));
#11636=CARTESIAN_POINT('',(0.,0.,0.));
#11637=CARTESIAN_POINT('',(0.,0.,0.));
#11638=CARTESIAN_POINT('',(0.,0.,0.));
#11639=CARTESIAN_POINT('',(0.,0.,0.));
#11640=CARTESIAN_POINT('',(0.,0.,0.));
#11641=CARTESIAN_POINT('',(0.,0.,0.));
#11642=CARTESIAN_POINT('',(0.,0.,0.));
#11643=CARTESIAN_POINT('',(0.,0.,0.));
#11644=CARTESIAN_POINT('',(-5.7,-1.5,2.2));
#11645=CARTESIAN_POINT('',(-5.7,1.5,2.2));
#11646=CARTESIAN_POINT('',(5.7,-1.5,2.2));
#11647=CARTESIAN_POINT('',(5.7,1.5,2.2));
#11648=CARTESIAN_POINT('',(0.,0.,6.53));
#11649=CARTESIAN_POINT('',(-4.75,0.,4.4));
#11650=CARTESIAN_POINT('',(-4.75,0.,4.56));
#11651=CARTESIAN_POINT('',(4.75,0.,4.4));
#11652=CARTESIAN_POINT('',(4.75,0.,4.56));
#11653=CARTESIAN_POINT('',(-5.7,14.5,2.2));
#11654=CARTESIAN_POINT('',(-5.7,17.5,2.2));
#11655=CARTESIAN_POINT('',(5.7,14.5,2.2));
#11656=CARTESIAN_POINT('',(5.7,17.5,2.2));
#11657=CARTESIAN_POINT('',(0.,16.,6.53));
#11658=CARTESIAN_POINT('',(-4.75,16.,4.4));
#11659=CARTESIAN_POINT('',(-4.75,16.,4.56));
#11660=CARTESIAN_POINT('',(4.75,16.,4.4));
#11661=CARTESIAN_POINT('',(4.75,16.,4.56));
#11662=CARTESIAN_POINT('',(5.6,-5.9,2.));
#11663=CARTESIAN_POINT('',(8.,-5.9,2.));
#11664=CARTESIAN_POINT('',(6.5,-2.7,10.));
#11665=CARTESIAN_POINT('',(8.3,-3.7,6.5));
#11666=CARTESIAN_POINT('',(0.,0.,0.));
#11667=CARTESIAN_POINT('',(0.,0.,0.));
#11668=CARTESIAN_POINT('',(0.,0.,0.));
#11669=CARTESIAN_POINT('',(0.,0.,0.));
#11670=CARTESIAN_POINT('',(0.,0.,0.));
#11671=CARTESIAN_POINT('',(0.,0.,0.));
#11672=CARTESIAN_POINT('',(0.,0.,0.));
#11673=CARTESIAN_POINT('',(0.,0.,0.));
#11674=CARTESIAN_POINT('',(0.,0.,0.));
#11675=CARTESIAN_POINT('',(0.,0.,0.));
#11676=CARTESIAN_POINT('',(0.,0.,0.));
#11677=CARTESIAN_POINT('',(0.,-1.25,8.33));
#11678=CARTESIAN_POINT('',(0.,18.85,8.33));
#11679=CARTESIAN_POINT('',(0.,3.5,8.33));
#11680=CARTESIAN_POINT('',(0.,12.5,8.33));
#11681=CARTESIAN_POINT('',(0.,-2.4,8.33));
#11682=CARTESIAN_POINT('',(0.,-6.,8.33));
#11683=CARTESIAN_POINT('',(0.,-5.7,10.03));
#11684=CARTESIAN_POINT('',(0.,0.,0.));
#11685=CARTESIAN_POINT('',(0.,0.,0.));
#11686=CARTESIAN_POINT('Origin',(6.5,-3.6,10.));
#11687=CARTESIAN_POINT('',(6.195,-3.5,10.));
#11688=CARTESIAN_POINT('Origin',(6.5,-3.5,10.));
#11689=CARTESIAN_POINT('',(6.195,-2.9,10.));
#11690=CARTESIAN_POINT('',(6.195,-3.6,10.));
#11691=CARTESIAN_POINT('Origin',(6.5,-2.9,10.));
#11692=CARTESIAN_POINT('Origin',(6.5,-3.5,10.));
#11693=CARTESIAN_POINT('',(5.96787188180707,-3.5,9.54520370952651));
#11694=CARTESIAN_POINT('',(5.96787188180707,-2.9,9.54520370952651));
#11695=CARTESIAN_POINT('',(5.96787188180707,-3.5,9.54520370952651));
#11696=CARTESIAN_POINT('',(6.83016839641497,-3.5,9.38275707374749));
#11697=CARTESIAN_POINT('Origin',(6.5,-3.5,10.));
#11698=CARTESIAN_POINT('',(6.83016839641497,-2.9,9.38275707374749));
#11699=CARTESIAN_POINT('',(6.83016839641497,-3.5,9.38275707374749));
#11700=CARTESIAN_POINT('Origin',(6.5,-2.9,10.));
#11701=CARTESIAN_POINT('Origin',(4.2,-3.5,6.53));
#11702=CARTESIAN_POINT('',(4.2,-2.9,6.53));
#11703=CARTESIAN_POINT('',(6.,-2.9,9.6));
#11704=CARTESIAN_POINT('',(4.2,-3.5,6.53));
#11705=CARTESIAN_POINT('',(4.2,-3.5,6.53));
#11706=CARTESIAN_POINT('',(6.,-3.5,9.6));
#11707=CARTESIAN_POINT('Origin',(5.6,-2.9,8.465));
#11708=CARTESIAN_POINT('',(4.6,-2.9,6.53));
#11709=CARTESIAN_POINT('',(4.6,-2.9,6.53));
#11710=CARTESIAN_POINT('',(4.2,-2.9,6.53));
#11711=CARTESIAN_POINT('Origin',(4.6,-3.5,6.53));
#11712=CARTESIAN_POINT('',(4.6,-3.5,6.53));
#11713=CARTESIAN_POINT('',(4.2,-3.5,6.53));
#11714=CARTESIAN_POINT('',(4.6,-3.5,6.53));
#11715=CARTESIAN_POINT('Origin',(7.,-3.5,9.6));
#11716=CARTESIAN_POINT('',(4.6,-3.5,6.53));
#11717=CARTESIAN_POINT('Origin',(5.6,-3.5,8.465));
#11718=CARTESIAN_POINT('',(0.,0.,0.));
#11719=CARTESIAN_POINT('',(0.,0.,0.));
#11720=CARTESIAN_POINT('',(0.,0.,0.));
#11721=CARTESIAN_POINT('',(0.,0.,0.));
#11722=UNCERTAINTY_MEASURE_WITH_UNIT(LENGTH_MEASURE(0.001),#11802,
'DISTANCE_ACCURACY_VALUE',
'Maximum model space distance between geometric entities at asserted c
onnectivities');
#11723=UNCERTAINTY_MEASURE_WITH_UNIT(LENGTH_MEASURE(0.001),#11802,
'DISTANCE_ACCURACY_VALUE',
'Maximum model space distance between geometric entities at asserted c
onnectivities');
#11724=UNCERTAINTY_MEASURE_WITH_UNIT(LENGTH_MEASURE(0.001),#11802,
'DISTANCE_ACCURACY_VALUE',
'Maximum model space distance between geometric entities at asserted c
onnectivities');
#11725=UNCERTAINTY_MEASURE_WITH_UNIT(LENGTH_MEASURE(0.001),#11802,
'DISTANCE_ACCURACY_VALUE',
'Maximum model space distance between geometric entities at asserted c
onnectivities');
#11726=UNCERTAINTY_MEASURE_WITH_UNIT(LENGTH_MEASURE(0.001),#11802,
'DISTANCE_ACCURACY_VALUE',
'Maximum model space distance between geometric entities at asserted c
onnectivities');
#11727=UNCERTAINTY_MEASURE_WITH_UNIT(LENGTH_MEASURE(0.001),#11802,
'DISTANCE_ACCURACY_VALUE',
'Maximum model space distance between geometric entities at asserted c
onnectivities');
#11728=UNCERTAINTY_MEASURE_WITH_UNIT(LENGTH_MEASURE(0.001),#11802,
'DISTANCE_ACCURACY_VALUE',
'Maximum model space distance between geometric entities at asserted c
onnectivities');
#11729=UNCERTAINTY_MEASURE_WITH_UNIT(LENGTH_MEASURE(0.001),#11802,
'DISTANCE_ACCURACY_VALUE',
'Maximum model space distance between geometric entities at asserted c
onnectivities');
#11730=UNCERTAINTY_MEASURE_WITH_UNIT(LENGTH_MEASURE(0.001),#11802,
'DISTANCE_ACCURACY_VALUE',
'Maximum model space distance between geometric entities at asserted c
onnectivities');
#11731=UNCERTAINTY_MEASURE_WITH_UNIT(LENGTH_MEASURE(0.001),#11802,
'DISTANCE_ACCURACY_VALUE',
'Maximum model space distance between geometric entities at asserted c
onnectivities');
#11732=UNCERTAINTY_MEASURE_WITH_UNIT(LENGTH_MEASURE(0.001),#11802,
'DISTANCE_ACCURACY_VALUE',
'Maximum model space distance between geometric entities at asserted c
onnectivities');
#11733=UNCERTAINTY_MEASURE_WITH_UNIT(LENGTH_MEASURE(0.001),#11802,
'DISTANCE_ACCURACY_VALUE',
'Maximum model space distance between geometric entities at asserted c
onnectivities');
#11734=UNCERTAINTY_MEASURE_WITH_UNIT(LENGTH_MEASURE(0.001),#11802,
'DISTANCE_ACCURACY_VALUE',
'Maximum model space distance between geometric entities at asserted c
onnectivities');
#11735=UNCERTAINTY_MEASURE_WITH_UNIT(LENGTH_MEASURE(0.001),#11802,
'DISTANCE_ACCURACY_VALUE',
'Maximum model space distance between geometric entities at asserted c
onnectivities');
#11736=UNCERTAINTY_MEASURE_WITH_UNIT(LENGTH_MEASURE(0.001),#11802,
'DISTANCE_ACCURACY_VALUE',
'Maximum model space distance between geometric entities at asserted c
onnectivities');
#11737=UNCERTAINTY_MEASURE_WITH_UNIT(LENGTH_MEASURE(0.001),#11802,
'DISTANCE_ACCURACY_VALUE',
'Maximum model space distance between geometric entities at asserted c
onnectivities');
#11738=UNCERTAINTY_MEASURE_WITH_UNIT(LENGTH_MEASURE(0.001),#11802,
'DISTANCE_ACCURACY_VALUE',
'Maximum model space distance between geometric entities at asserted c
onnectivities');
#11739=UNCERTAINTY_MEASURE_WITH_UNIT(LENGTH_MEASURE(0.001),#11802,
'DISTANCE_ACCURACY_VALUE',
'Maximum model space distance between geometric entities at asserted c
onnectivities');
#11740=UNCERTAINTY_MEASURE_WITH_UNIT(LENGTH_MEASURE(0.001),#11802,
'DISTANCE_ACCURACY_VALUE',
'Maximum model space distance between geometric entities at asserted c
onnectivities');
#11741=UNCERTAINTY_MEASURE_WITH_UNIT(LENGTH_MEASURE(0.001),#11802,
'DISTANCE_ACCURACY_VALUE',
'Maximum model space distance between geometric entities at asserted c
onnectivities');
#11742=UNCERTAINTY_MEASURE_WITH_UNIT(LENGTH_MEASURE(0.001),#11802,
'DISTANCE_ACCURACY_VALUE',
'Maximum model space distance between geometric entities at asserted c
onnectivities');
#11743=UNCERTAINTY_MEASURE_WITH_UNIT(LENGTH_MEASURE(0.001),#11802,
'DISTANCE_ACCURACY_VALUE',
'Maximum model space distance between geometric entities at asserted c
onnectivities');
#11744=UNCERTAINTY_MEASURE_WITH_UNIT(LENGTH_MEASURE(0.001),#11802,
'DISTANCE_ACCURACY_VALUE',
'Maximum model space distance between geometric entities at asserted c
onnectivities');
#11745=UNCERTAINTY_MEASURE_WITH_UNIT(LENGTH_MEASURE(0.001),#11802,
'DISTANCE_ACCURACY_VALUE',
'Maximum model space distance between geometric entities at asserted c
onnectivities');
#11746=UNCERTAINTY_MEASURE_WITH_UNIT(LENGTH_MEASURE(0.001),#11802,
'DISTANCE_ACCURACY_VALUE',
'Maximum model space distance between geometric entities at asserted c
onnectivities');
#11747=UNCERTAINTY_MEASURE_WITH_UNIT(LENGTH_MEASURE(0.001),#11802,
'DISTANCE_ACCURACY_VALUE',
'Maximum model space distance between geometric entities at asserted c
onnectivities');
#11748=UNCERTAINTY_MEASURE_WITH_UNIT(LENGTH_MEASURE(0.001),#11802,
'DISTANCE_ACCURACY_VALUE',
'Maximum model space distance between geometric entities at asserted c
onnectivities');
#11749=UNCERTAINTY_MEASURE_WITH_UNIT(LENGTH_MEASURE(0.001),#11802,
'DISTANCE_ACCURACY_VALUE',
'Maximum model space distance between geometric entities at asserted c
onnectivities');
#11750=UNCERTAINTY_MEASURE_WITH_UNIT(LENGTH_MEASURE(0.001),#11802,
'DISTANCE_ACCURACY_VALUE',
'Maximum model space distance between geometric entities at asserted c
onnectivities');
#11751=UNCERTAINTY_MEASURE_WITH_UNIT(LENGTH_MEASURE(0.001),#11802,
'DISTANCE_ACCURACY_VALUE',
'Maximum model space distance between geometric entities at asserted c
onnectivities');
#11752=UNCERTAINTY_MEASURE_WITH_UNIT(LENGTH_MEASURE(0.001),#11802,
'DISTANCE_ACCURACY_VALUE',
'Maximum model space distance between geometric entities at asserted c
onnectivities');
#11753=UNCERTAINTY_MEASURE_WITH_UNIT(LENGTH_MEASURE(0.001),#11802,
'DISTANCE_ACCURACY_VALUE',
'Maximum model space distance between geometric entities at asserted c
onnectivities');
#11754=UNCERTAINTY_MEASURE_WITH_UNIT(LENGTH_MEASURE(0.001),#11802,
'DISTANCE_ACCURACY_VALUE',
'Maximum model space distance between geometric entities at asserted c
onnectivities');
#11755=UNCERTAINTY_MEASURE_WITH_UNIT(LENGTH_MEASURE(0.001),#11802,
'DISTANCE_ACCURACY_VALUE',
'Maximum model space distance between geometric entities at asserted c
onnectivities');
#11756=UNCERTAINTY_MEASURE_WITH_UNIT(LENGTH_MEASURE(0.001),#11802,
'DISTANCE_ACCURACY_VALUE',
'Maximum model space distance between geometric entities at asserted c
onnectivities');
#11757=UNCERTAINTY_MEASURE_WITH_UNIT(LENGTH_MEASURE(0.001),#11802,
'DISTANCE_ACCURACY_VALUE',
'Maximum model space distance between geometric entities at asserted c
onnectivities');
#11758=UNCERTAINTY_MEASURE_WITH_UNIT(LENGTH_MEASURE(0.001),#11802,
'DISTANCE_ACCURACY_VALUE',
'Maximum model space distance between geometric entities at asserted c
onnectivities');
#11759=UNCERTAINTY_MEASURE_WITH_UNIT(LENGTH_MEASURE(0.001),#11802,
'DISTANCE_ACCURACY_VALUE',
'Maximum model space distance between geometric entities at asserted c
onnectivities');
#11760=UNCERTAINTY_MEASURE_WITH_UNIT(LENGTH_MEASURE(0.001),#11802,
'DISTANCE_ACCURACY_VALUE',
'Maximum model space distance between geometric entities at asserted c
onnectivities');
#11761=UNCERTAINTY_MEASURE_WITH_UNIT(LENGTH_MEASURE(0.001),#11802,
'DISTANCE_ACCURACY_VALUE',
'Maximum model space distance between geometric entities at asserted c
onnectivities');
#11762=(
GEOMETRIC_REPRESENTATION_CONTEXT(3)
GLOBAL_UNCERTAINTY_ASSIGNED_CONTEXT((#11722))
GLOBAL_UNIT_ASSIGNED_CONTEXT((#11802,#11804,#11805))
REPRESENTATION_CONTEXT('','3D')
);
#11763=(
GEOMETRIC_REPRESENTATION_CONTEXT(3)
GLOBAL_UNCERTAINTY_ASSIGNED_CONTEXT((#11723))
GLOBAL_UNIT_ASSIGNED_CONTEXT((#11802,#11804,#11805))
REPRESENTATION_CONTEXT('','3D')
);
#11764=(
GEOMETRIC_REPRESENTATION_CONTEXT(3)
GLOBAL_UNCERTAINTY_ASSIGNED_CONTEXT((#11724))
GLOBAL_UNIT_ASSIGNED_CONTEXT((#11802,#11804,#11805))
REPRESENTATION_CONTEXT('','3D')
);
#11765=(
GEOMETRIC_REPRESENTATION_CONTEXT(3)
GLOBAL_UNCERTAINTY_ASSIGNED_CONTEXT((#11725))
GLOBAL_UNIT_ASSIGNED_CONTEXT((#11802,#11804,#11805))
REPRESENTATION_CONTEXT('','3D')
);
#11766=(
GEOMETRIC_REPRESENTATION_CONTEXT(3)
GLOBAL_UNCERTAINTY_ASSIGNED_CONTEXT((#11726))
GLOBAL_UNIT_ASSIGNED_CONTEXT((#11802,#11804,#11805))
REPRESENTATION_CONTEXT('','3D')
);
#11767=(
GEOMETRIC_REPRESENTATION_CONTEXT(3)
GLOBAL_UNCERTAINTY_ASSIGNED_CONTEXT((#11727))
GLOBAL_UNIT_ASSIGNED_CONTEXT((#11802,#11804,#11805))
REPRESENTATION_CONTEXT('','3D')
);
#11768=(
GEOMETRIC_REPRESENTATION_CONTEXT(3)
GLOBAL_UNCERTAINTY_ASSIGNED_CONTEXT((#11728))
GLOBAL_UNIT_ASSIGNED_CONTEXT((#11802,#11804,#11805))
REPRESENTATION_CONTEXT('','3D')
);
#11769=(
GEOMETRIC_REPRESENTATION_CONTEXT(3)
GLOBAL_UNCERTAINTY_ASSIGNED_CONTEXT((#11729))
GLOBAL_UNIT_ASSIGNED_CONTEXT((#11802,#11804,#11805))
REPRESENTATION_CONTEXT('','3D')
);
#11770=(
GEOMETRIC_REPRESENTATION_CONTEXT(3)
GLOBAL_UNCERTAINTY_ASSIGNED_CONTEXT((#11730))
GLOBAL_UNIT_ASSIGNED_CONTEXT((#11802,#11804,#11805))
REPRESENTATION_CONTEXT('','3D')
);
#11771=(
GEOMETRIC_REPRESENTATION_CONTEXT(3)
GLOBAL_UNCERTAINTY_ASSIGNED_CONTEXT((#11731))
GLOBAL_UNIT_ASSIGNED_CONTEXT((#11802,#11804,#11805))
REPRESENTATION_CONTEXT('','3D')
);
#11772=(
GEOMETRIC_REPRESENTATION_CONTEXT(3)
GLOBAL_UNCERTAINTY_ASSIGNED_CONTEXT((#11732))
GLOBAL_UNIT_ASSIGNED_CONTEXT((#11802,#11804,#11805))
REPRESENTATION_CONTEXT('','3D')
);
#11773=(
GEOMETRIC_REPRESENTATION_CONTEXT(3)
GLOBAL_UNCERTAINTY_ASSIGNED_CONTEXT((#11733))
GLOBAL_UNIT_ASSIGNED_CONTEXT((#11802,#11804,#11805))
REPRESENTATION_CONTEXT('','3D')
);
#11774=(
GEOMETRIC_REPRESENTATION_CONTEXT(3)
GLOBAL_UNCERTAINTY_ASSIGNED_CONTEXT((#11734))
GLOBAL_UNIT_ASSIGNED_CONTEXT((#11802,#11804,#11805))
REPRESENTATION_CONTEXT('','3D')
);
#11775=(
GEOMETRIC_REPRESENTATION_CONTEXT(3)
GLOBAL_UNCERTAINTY_ASSIGNED_CONTEXT((#11735))
GLOBAL_UNIT_ASSIGNED_CONTEXT((#11802,#11804,#11805))
REPRESENTATION_CONTEXT('','3D')
);
#11776=(
GEOMETRIC_REPRESENTATION_CONTEXT(3)
GLOBAL_UNCERTAINTY_ASSIGNED_CONTEXT((#11736))
GLOBAL_UNIT_ASSIGNED_CONTEXT((#11802,#11804,#11805))
REPRESENTATION_CONTEXT('','3D')
);
#11777=(
GEOMETRIC_REPRESENTATION_CONTEXT(3)
GLOBAL_UNCERTAINTY_ASSIGNED_CONTEXT((#11737))
GLOBAL_UNIT_ASSIGNED_CONTEXT((#11802,#11804,#11805))
REPRESENTATION_CONTEXT('','3D')
);
#11778=(
GEOMETRIC_REPRESENTATION_CONTEXT(3)
GLOBAL_UNCERTAINTY_ASSIGNED_CONTEXT((#11738))
GLOBAL_UNIT_ASSIGNED_CONTEXT((#11802,#11804,#11805))
REPRESENTATION_CONTEXT('','3D')
);
#11779=(
GEOMETRIC_REPRESENTATION_CONTEXT(3)
GLOBAL_UNCERTAINTY_ASSIGNED_CONTEXT((#11739))
GLOBAL_UNIT_ASSIGNED_CONTEXT((#11802,#11804,#11805))
REPRESENTATION_CONTEXT('','3D')
);
#11780=(
GEOMETRIC_REPRESENTATION_CONTEXT(3)
GLOBAL_UNCERTAINTY_ASSIGNED_CONTEXT((#11740))
GLOBAL_UNIT_ASSIGNED_CONTEXT((#11802,#11804,#11805))
REPRESENTATION_CONTEXT('','3D')
);
#11781=(
GEOMETRIC_REPRESENTATION_CONTEXT(3)
GLOBAL_UNCERTAINTY_ASSIGNED_CONTEXT((#11741))
GLOBAL_UNIT_ASSIGNED_CONTEXT((#11802,#11804,#11805))
REPRESENTATION_CONTEXT('','3D')
);
#11782=(
GEOMETRIC_REPRESENTATION_CONTEXT(3)
GLOBAL_UNCERTAINTY_ASSIGNED_CONTEXT((#11742))
GLOBAL_UNIT_ASSIGNED_CONTEXT((#11802,#11804,#11805))
REPRESENTATION_CONTEXT('','3D')
);
#11783=(
GEOMETRIC_REPRESENTATION_CONTEXT(3)
GLOBAL_UNCERTAINTY_ASSIGNED_CONTEXT((#11743))
GLOBAL_UNIT_ASSIGNED_CONTEXT((#11802,#11804,#11805))
REPRESENTATION_CONTEXT('','3D')
);
#11784=(
GEOMETRIC_REPRESENTATION_CONTEXT(3)
GLOBAL_UNCERTAINTY_ASSIGNED_CONTEXT((#11744))
GLOBAL_UNIT_ASSIGNED_CONTEXT((#11802,#11804,#11805))
REPRESENTATION_CONTEXT('','3D')
);
#11785=(
GEOMETRIC_REPRESENTATION_CONTEXT(3)
GLOBAL_UNCERTAINTY_ASSIGNED_CONTEXT((#11745))
GLOBAL_UNIT_ASSIGNED_CONTEXT((#11802,#11804,#11805))
REPRESENTATION_CONTEXT('','3D')
);
#11786=(
GEOMETRIC_REPRESENTATION_CONTEXT(3)
GLOBAL_UNCERTAINTY_ASSIGNED_CONTEXT((#11746))
GLOBAL_UNIT_ASSIGNED_CONTEXT((#11802,#11804,#11805))
REPRESENTATION_CONTEXT('','3D')
);
#11787=(
GEOMETRIC_REPRESENTATION_CONTEXT(3)
GLOBAL_UNCERTAINTY_ASSIGNED_CONTEXT((#11747))
GLOBAL_UNIT_ASSIGNED_CONTEXT((#11802,#11804,#11805))
REPRESENTATION_CONTEXT('','3D')
);
#11788=(
GEOMETRIC_REPRESENTATION_CONTEXT(3)
GLOBAL_UNCERTAINTY_ASSIGNED_CONTEXT((#11748))
GLOBAL_UNIT_ASSIGNED_CONTEXT((#11802,#11804,#11805))
REPRESENTATION_CONTEXT('','3D')
);
#11789=(
GEOMETRIC_REPRESENTATION_CONTEXT(3)
GLOBAL_UNCERTAINTY_ASSIGNED_CONTEXT((#11749))
GLOBAL_UNIT_ASSIGNED_CONTEXT((#11802,#11804,#11805))
REPRESENTATION_CONTEXT('','3D')
);
#11790=(
GEOMETRIC_REPRESENTATION_CONTEXT(3)
GLOBAL_UNCERTAINTY_ASSIGNED_CONTEXT((#11750))
GLOBAL_UNIT_ASSIGNED_CONTEXT((#11802,#11804,#11805))
REPRESENTATION_CONTEXT('','3D')
);
#11791=(
GEOMETRIC_REPRESENTATION_CONTEXT(3)
GLOBAL_UNCERTAINTY_ASSIGNED_CONTEXT((#11751))
GLOBAL_UNIT_ASSIGNED_CONTEXT((#11802,#11804,#11805))
REPRESENTATION_CONTEXT('','3D')
);
#11792=(
GEOMETRIC_REPRESENTATION_CONTEXT(3)
GLOBAL_UNCERTAINTY_ASSIGNED_CONTEXT((#11752))
GLOBAL_UNIT_ASSIGNED_CONTEXT((#11802,#11804,#11805))
REPRESENTATION_CONTEXT('','3D')
);
#11793=(
GEOMETRIC_REPRESENTATION_CONTEXT(3)
GLOBAL_UNCERTAINTY_ASSIGNED_CONTEXT((#11753))
GLOBAL_UNIT_ASSIGNED_CONTEXT((#11802,#11804,#11805))
REPRESENTATION_CONTEXT('','3D')
);
#11794=(
GEOMETRIC_REPRESENTATION_CONTEXT(3)
GLOBAL_UNCERTAINTY_ASSIGNED_CONTEXT((#11754))
GLOBAL_UNIT_ASSIGNED_CONTEXT((#11802,#11804,#11805))
REPRESENTATION_CONTEXT('','3D')
);
#11795=(
GEOMETRIC_REPRESENTATION_CONTEXT(3)
GLOBAL_UNCERTAINTY_ASSIGNED_CONTEXT((#11755))
GLOBAL_UNIT_ASSIGNED_CONTEXT((#11802,#11804,#11805))
REPRESENTATION_CONTEXT('','3D')
);
#11796=(
GEOMETRIC_REPRESENTATION_CONTEXT(3)
GLOBAL_UNCERTAINTY_ASSIGNED_CONTEXT((#11756))
GLOBAL_UNIT_ASSIGNED_CONTEXT((#11802,#11804,#11805))
REPRESENTATION_CONTEXT('','3D')
);
#11797=(
GEOMETRIC_REPRESENTATION_CONTEXT(3)
GLOBAL_UNCERTAINTY_ASSIGNED_CONTEXT((#11757))
GLOBAL_UNIT_ASSIGNED_CONTEXT((#11802,#11804,#11805))
REPRESENTATION_CONTEXT('','3D')
);
#11798=(
GEOMETRIC_REPRESENTATION_CONTEXT(3)
GLOBAL_UNCERTAINTY_ASSIGNED_CONTEXT((#11758))
GLOBAL_UNIT_ASSIGNED_CONTEXT((#11802,#11804,#11805))
REPRESENTATION_CONTEXT('','3D')
);
#11799=(
GEOMETRIC_REPRESENTATION_CONTEXT(3)
GLOBAL_UNCERTAINTY_ASSIGNED_CONTEXT((#11759))
GLOBAL_UNIT_ASSIGNED_CONTEXT((#11802,#11804,#11805))
REPRESENTATION_CONTEXT('','3D')
);
#11800=(
GEOMETRIC_REPRESENTATION_CONTEXT(3)
GLOBAL_UNCERTAINTY_ASSIGNED_CONTEXT((#11760))
GLOBAL_UNIT_ASSIGNED_CONTEXT((#11802,#11804,#11805))
REPRESENTATION_CONTEXT('','3D')
);
#11801=(
GEOMETRIC_REPRESENTATION_CONTEXT(3)
GLOBAL_UNCERTAINTY_ASSIGNED_CONTEXT((#11761))
GLOBAL_UNIT_ASSIGNED_CONTEXT((#11802,#11804,#11805))
REPRESENTATION_CONTEXT('','3D')
);
#11802=(
LENGTH_UNIT()
NAMED_UNIT(*)
SI_UNIT(.CENTI.,.METRE.)
);
#11803=(
LENGTH_UNIT()
NAMED_UNIT(*)
SI_UNIT($,.METRE.)
);
#11804=(
NAMED_UNIT(*)
PLANE_ANGLE_UNIT()
SI_UNIT($,.RADIAN.)
);
#11805=(
NAMED_UNIT(*)
SI_UNIT($,.STERADIAN.)
SOLID_ANGLE_UNIT()
);
#11806=SHAPE_DEFINITION_REPRESENTATION(#11845,#11945);
#11807=SHAPE_DEFINITION_REPRESENTATION(#11846,#11946);
#11808=SHAPE_DEFINITION_REPRESENTATION(#11847,#11947);
#11809=SHAPE_DEFINITION_REPRESENTATION(#11848,#11948);
#11810=SHAPE_DEFINITION_REPRESENTATION(#11849,#11949);
#11811=SHAPE_DEFINITION_REPRESENTATION(#11850,#11950);
#11812=SHAPE_DEFINITION_REPRESENTATION(#11851,#11951);
#11813=SHAPE_DEFINITION_REPRESENTATION(#11852,#11952);
#11814=SHAPE_DEFINITION_REPRESENTATION(#11853,#11953);
#11815=SHAPE_DEFINITION_REPRESENTATION(#11854,#11954);
#11816=SHAPE_DEFINITION_REPRESENTATION(#11855,#11955);
#11817=SHAPE_DEFINITION_REPRESENTATION(#11856,#11956);
#11818=SHAPE_DEFINITION_REPRESENTATION(#11857,#11957);
#11819=SHAPE_DEFINITION_REPRESENTATION(#11858,#11958);
#11820=SHAPE_DEFINITION_REPRESENTATION(#11859,#11959);
#11821=SHAPE_DEFINITION_REPRESENTATION(#11860,#11960);
#11822=SHAPE_DEFINITION_REPRESENTATION(#11861,#11961);
#11823=SHAPE_DEFINITION_REPRESENTATION(#11862,#11962);
#11824=SHAPE_DEFINITION_REPRESENTATION(#11863,#11963);
#11825=SHAPE_DEFINITION_REPRESENTATION(#11864,#11964);
#11826=SHAPE_DEFINITION_REPRESENTATION(#11867,#11965);
#11827=SHAPE_DEFINITION_REPRESENTATION(#11868,#11966);
#11828=SHAPE_DEFINITION_REPRESENTATION(#11869,#11967);
#11829=SHAPE_DEFINITION_REPRESENTATION(#11870,#11968);
#11830=SHAPE_DEFINITION_REPRESENTATION(#11871,#11969);
#11831=SHAPE_DEFINITION_REPRESENTATION(#11872,#11970);
#11832=SHAPE_DEFINITION_REPRESENTATION(#11873,#11971);
#11833=SHAPE_DEFINITION_REPRESENTATION(#11874,#11972);
#11834=SHAPE_DEFINITION_REPRESENTATION(#11875,#11973);
#11835=SHAPE_DEFINITION_REPRESENTATION(#11876,#11974);
#11836=SHAPE_DEFINITION_REPRESENTATION(#11877,#11975);
#11837=SHAPE_DEFINITION_REPRESENTATION(#11878,#11976);
#11838=SHAPE_DEFINITION_REPRESENTATION(#11879,#11977);
#11839=SHAPE_DEFINITION_REPRESENTATION(#11880,#11978);
#11840=SHAPE_DEFINITION_REPRESENTATION(#11881,#11979);
#11841=SHAPE_DEFINITION_REPRESENTATION(#11882,#11980);
#11842=SHAPE_DEFINITION_REPRESENTATION(#11883,#11981);
#11843=SHAPE_DEFINITION_REPRESENTATION(#11939,#11982);
#11844=SHAPE_DEFINITION_REPRESENTATION(#11940,#11983);
#11845=PRODUCT_DEFINITION_SHAPE('',$,#11985);
#11846=PRODUCT_DEFINITION_SHAPE('',$,#11986);
#11847=PRODUCT_DEFINITION_SHAPE('',$,#11987);
#11848=PRODUCT_DEFINITION_SHAPE('',$,#11988);
#11849=PRODUCT_DEFINITION_SHAPE('',$,#11989);
#11850=PRODUCT_DEFINITION_SHAPE('',$,#11990);
#11851=PRODUCT_DEFINITION_SHAPE('',$,#11991);
#11852=PRODUCT_DEFINITION_SHAPE('',$,#11992);
#11853=PRODUCT_DEFINITION_SHAPE('',$,#11993);
#11854=PRODUCT_DEFINITION_SHAPE('',$,#11994);
#11855=PRODUCT_DEFINITION_SHAPE('',$,#11995);
#11856=PRODUCT_DEFINITION_SHAPE('',$,#11996);
#11857=PRODUCT_DEFINITION_SHAPE('',$,#11997);
#11858=PRODUCT_DEFINITION_SHAPE('',$,#11998);
#11859=PRODUCT_DEFINITION_SHAPE('',$,#11999);
#11860=PRODUCT_DEFINITION_SHAPE('',$,#12000);
#11861=PRODUCT_DEFINITION_SHAPE('',$,#12001);
#11862=PRODUCT_DEFINITION_SHAPE('',$,#12002);
#11863=PRODUCT_DEFINITION_SHAPE('',$,#12003);
#11864=PRODUCT_DEFINITION_SHAPE('',$,#12004);
#11865=PRODUCT_DEFINITION_SHAPE($,$,#212);
#11866=PRODUCT_DEFINITION_SHAPE($,$,#213);
#11867=PRODUCT_DEFINITION_SHAPE('',$,#12005);
#11868=PRODUCT_DEFINITION_SHAPE('',$,#12006);
#11869=PRODUCT_DEFINITION_SHAPE('',$,#12007);
#11870=PRODUCT_DEFINITION_SHAPE('',$,#12008);
#11871=PRODUCT_DEFINITION_SHAPE('',$,#12009);
#11872=PRODUCT_DEFINITION_SHAPE('',$,#12010);
#11873=PRODUCT_DEFINITION_SHAPE('',$,#12011);
#11874=PRODUCT_DEFINITION_SHAPE('',$,#12012);
#11875=PRODUCT_DEFINITION_SHAPE('',$,#12013);
#11876=PRODUCT_DEFINITION_SHAPE('',$,#12014);
#11877=PRODUCT_DEFINITION_SHAPE('',$,#12015);
#11878=PRODUCT_DEFINITION_SHAPE('',$,#12016);
#11879=PRODUCT_DEFINITION_SHAPE('',$,#12017);
#11880=PRODUCT_DEFINITION_SHAPE('',$,#12018);
#11881=PRODUCT_DEFINITION_SHAPE('',$,#12019);
#11882=PRODUCT_DEFINITION_SHAPE('',$,#12020);
#11883=PRODUCT_DEFINITION_SHAPE('',$,#12021);
#11884=PRODUCT_DEFINITION_SHAPE($,$,#214);
#11885=PRODUCT_DEFINITION_SHAPE($,$,#215);
#11886=PRODUCT_DEFINITION_SHAPE($,$,#216);
#11887=PRODUCT_DEFINITION_SHAPE($,$,#217);
#11888=PRODUCT_DEFINITION_SHAPE($,$,#218);
#11889=PRODUCT_DEFINITION_SHAPE($,$,#219);
#11890=PRODUCT_DEFINITION_SHAPE($,$,#220);
#11891=PRODUCT_DEFINITION_SHAPE($,$,#221);
#11892=PRODUCT_DEFINITION_SHAPE($,$,#222);
#11893=PRODUCT_DEFINITION_SHAPE($,$,#223);
#11894=PRODUCT_DEFINITION_SHAPE($,$,#224);
#11895=PRODUCT_DEFINITION_SHAPE($,$,#225);
#11896=PRODUCT_DEFINITION_SHAPE($,$,#226);
#11897=PRODUCT_DEFINITION_SHAPE($,$,#227);
#11898=PRODUCT_DEFINITION_SHAPE($,$,#228);
#11899=PRODUCT_DEFINITION_SHAPE($,$,#229);
#11900=PRODUCT_DEFINITION_SHAPE($,$,#230);
#11901=PRODUCT_DEFINITION_SHAPE($,$,#231);
#11902=PRODUCT_DEFINITION_SHAPE($,$,#232);
#11903=PRODUCT_DEFINITION_SHAPE($,$,#233);
#11904=PRODUCT_DEFINITION_SHAPE($,$,#234);
#11905=PRODUCT_DEFINITION_SHAPE($,$,#235);
#11906=PRODUCT_DEFINITION_SHAPE($,$,#236);
#11907=PRODUCT_DEFINITION_SHAPE($,$,#237);
#11908=PRODUCT_DEFINITION_SHAPE($,$,#238);
#11909=PRODUCT_DEFINITION_SHAPE($,$,#239);
#11910=PRODUCT_DEFINITION_SHAPE($,$,#240);
#11911=PRODUCT_DEFINITION_SHAPE($,$,#241);
#11912=PRODUCT_DEFINITION_SHAPE($,$,#242);
#11913=PRODUCT_DEFINITION_SHAPE($,$,#243);
#11914=PRODUCT_DEFINITION_SHAPE($,$,#244);
#11915=PRODUCT_DEFINITION_SHAPE($,$,#245);
#11916=PRODUCT_DEFINITION_SHAPE($,$,#246);
#11917=PRODUCT_DEFINITION_SHAPE($,$,#247);
#11918=PRODUCT_DEFINITION_SHAPE($,$,#248);
#11919=PRODUCT_DEFINITION_SHAPE($,$,#249);
#11920=PRODUCT_DEFINITION_SHAPE($,$,#250);
#11921=PRODUCT_DEFINITION_SHAPE($,$,#251);
#11922=PRODUCT_DEFINITION_SHAPE($,$,#252);
#11923=PRODUCT_DEFINITION_SHAPE($,$,#253);
#11924=PRODUCT_DEFINITION_SHAPE($,$,#254);
#11925=PRODUCT_DEFINITION_SHAPE($,$,#255);
#11926=PRODUCT_DEFINITION_SHAPE($,$,#256);
#11927=PRODUCT_DEFINITION_SHAPE($,$,#257);
#11928=PRODUCT_DEFINITION_SHAPE($,$,#258);
#11929=PRODUCT_DEFINITION_SHAPE($,$,#259);
#11930=PRODUCT_DEFINITION_SHAPE($,$,#260);
#11931=PRODUCT_DEFINITION_SHAPE($,$,#261);
#11932=PRODUCT_DEFINITION_SHAPE($,$,#262);
#11933=PRODUCT_DEFINITION_SHAPE($,$,#263);
#11934=PRODUCT_DEFINITION_SHAPE($,$,#264);
#11935=PRODUCT_DEFINITION_SHAPE($,$,#265);
#11936=PRODUCT_DEFINITION_SHAPE($,$,#266);
#11937=PRODUCT_DEFINITION_SHAPE($,$,#267);
#11938=PRODUCT_DEFINITION_SHAPE($,$,#268);
#11939=PRODUCT_DEFINITION_SHAPE('',$,#12022);
#11940=PRODUCT_DEFINITION_SHAPE('',$,#12023);
#11941=PRODUCT_DEFINITION_SHAPE($,$,#269);
#11942=PRODUCT_DEFINITION_SHAPE($,$,#270);
#11943=PRODUCT_DEFINITION_SHAPE($,$,#271);
#11944=PRODUCT_DEFINITION_SHAPE($,$,#272);
#11945=SHAPE_REPRESENTATION('',(#6679,#7355,#7356,#7357),#11762);
#11946=SHAPE_REPRESENTATION('',(#6680,#7286,#7287,#7288,#7289,#7290,#7291,
#7292,#7293,#7294,#7295,#7296,#7297,#7298,#7299,#7300,#7301,#7302,#7303,
#7304,#7305,#7306,#7307,#7308,#7309,#7310,#7311,#7312,#7313,#7314,#7315,
#7316,#7317,#7318,#7319,#7320,#7321,#7322),#11763);
#11947=SHAPE_REPRESENTATION('',(#6681),#11764);
#11948=SHAPE_REPRESENTATION('',(#6718),#11765);
#11949=SHAPE_REPRESENTATION('',(#6725),#11766);
#11950=SHAPE_REPRESENTATION('',(#6732),#11767);
#11951=SHAPE_REPRESENTATION('',(#6773),#11768);
#11952=SHAPE_REPRESENTATION('',(#6782),#11769);
#11953=SHAPE_REPRESENTATION('',(#6791),#11770);
#11954=SHAPE_REPRESENTATION('',(#6832),#11771);
#11955=SHAPE_REPRESENTATION('',(#6841),#11772);
#11956=SHAPE_REPRESENTATION('',(#6850),#11773);
#11957=SHAPE_REPRESENTATION('',(#6871),#11774);
#11958=SHAPE_REPRESENTATION('',(#6885),#11775);
#11959=SHAPE_REPRESENTATION('',(#6894),#11776);
#11960=SHAPE_REPRESENTATION('',(#6903),#11777);
#11961=SHAPE_REPRESENTATION('',(#6910),#11778);
#11962=SHAPE_REPRESENTATION('',(#6920,#6990,#6991),#11779);
#11963=SHAPE_REPRESENTATION('',(#6921),#11780);
#11964=SHAPE_REPRESENTATION('',(#6962),#11781);
#11965=SHAPE_REPRESENTATION('',(#6992),#11782);
#11966=SHAPE_REPRESENTATION('',(#7001),#11783);
#11967=SHAPE_REPRESENTATION('',(#7025),#11784);
#11968=SHAPE_REPRESENTATION('',(#7049,#7323,#7324,#7325,#7326,#7327,#7328,
#7329,#7330,#7331,#7332,#7333,#7334,#7335,#7336,#7337,#7338,#7339,#7340),
#11785);
#11969=SHAPE_REPRESENTATION('',(#7050),#11786);
#11970=SHAPE_REPRESENTATION('',(#7056),#11787);
#11971=SHAPE_REPRESENTATION('',(#7071),#11788);
#11972=SHAPE_REPRESENTATION('',(#7086),#11789);
#11973=SHAPE_REPRESENTATION('',(#7095),#11790);
#11974=SHAPE_REPRESENTATION('',(#7104),#11791);
#11975=SHAPE_REPRESENTATION('',(#7119),#11792);
#11976=SHAPE_REPRESENTATION('',(#7128),#11793);
#11977=SHAPE_REPRESENTATION('',(#7143),#11794);
#11978=SHAPE_REPRESENTATION('',(#7207),#11795);
#11979=SHAPE_REPRESENTATION('',(#7233),#11796);
#11980=SHAPE_REPRESENTATION('',(#7243),#11797);
#11981=SHAPE_REPRESENTATION('',(#7260),#11798);
#11982=SHAPE_REPRESENTATION('',(#7341,#7354),#11799);
#11983=SHAPE_REPRESENTATION('',(#7342),#11800);
#11984=PRODUCT_DEFINITION_CONTEXT('part definition',#12103,'design');
#11985=PRODUCT_DEFINITION('PAT-086',
'PAT-086',#12024,#11984);
#11986=PRODUCT_DEFINITION('Base and bearing supports',
'Base and bearing supports',#12025,#11984);
#11987=PRODUCT_DEFINITION('Base','Base',#12026,#11984);
#11988=PRODUCT_DEFINITION('Foot','Foot',#12027,#11984);
#11989=PRODUCT_DEFINITION('Foot (1)','Foot (1)',#12028,#11984);
#11990=PRODUCT_DEFINITION('Bearing riser','Bearing riser',#12029,#11984);
#11991=PRODUCT_DEFINITION('Mounting bush','Mounting bush',#12030,#11984);
#11992=PRODUCT_DEFINITION('Mounting bush (1)','Mounting bush (1)',#12031,
#11984);
#11993=PRODUCT_DEFINITION('Bearing riser (1)','Bearing riser (1)',#12032,
#11984);
#11994=PRODUCT_DEFINITION('Mounting bush (2)','Mounting bush (2)',#12033,
#11984);
#11995=PRODUCT_DEFINITION('Mounting bush (3)','Mounting bush (3)',#12034,
#11984);
#11996=PRODUCT_DEFINITION('Pawl pedestal','Pawl pedestal',#12035,#11984);
#11997=PRODUCT_DEFINITION('Pawl pivot pin','Pawl pivot pin',#12036,#11984);
#11998=PRODUCT_DEFINITION('Pawl pivot sleeve','Pawl pivot sleeve',#12037,
#11984);
#11999=PRODUCT_DEFINITION('Pawl pin keeper','Pawl pin keeper',#12038,#11984);
#12000=PRODUCT_DEFINITION('Pawl leaf spring','Pawl leaf spring',#12039,
#11984);
#12001=PRODUCT_DEFINITION('Spring anchor','Spring anchor',#12040,#11984);
#12002=PRODUCT_DEFINITION('Pillow Block Bearing - 20 mm Bore',
'Pillow Block Bearing - 20 mm Bore',#12041,#11984);
#12003=PRODUCT_DEFINITION('Housing','Housing',#12042,#11984);
#12004=PRODUCT_DEFINITION('Insert bearing','Insert bearing',#12043,#11984);
#12005=PRODUCT_DEFINITION('Flat Washer - M8','Flat Washer - M8',#12044,
#11984);
#12006=PRODUCT_DEFINITION('M8x25 Bolt','M8x25 Bolt',#12045,#11984);
#12007=PRODUCT_DEFINITION('M4x10 Cap Screw','M4x10 Cap Screw',#12046,#11984);
#12008=PRODUCT_DEFINITION('Drum shaft and crank','Drum shaft and crank',
#12047,#11984);
#12009=PRODUCT_DEFINITION('Drum shaft','Drum shaft',#12048,#11984);
#12010=PRODUCT_DEFINITION('Shaft collar','Shaft collar',#12049,#11984);
#12011=PRODUCT_DEFINITION('Shaft collar (1)','Shaft collar (1)',#12050,#11984);
#12012=PRODUCT_DEFINITION('Winding drum','Winding drum',#12051,#11984);
#12013=PRODUCT_DEFINITION('Drum flange','Drum flange',#12052,#11984);
#12014=PRODUCT_DEFINITION('Drum hub','Drum hub',#12053,#11984);
#12015=PRODUCT_DEFINITION('Drum flange (1)','Drum flange (1)',#12054,#11984);
#12016=PRODUCT_DEFINITION('Drum hub (1)','Drum hub (1)',#12055,#11984);
#12017=PRODUCT_DEFINITION('Ratchet wheel','Ratchet wheel',#12056,#11984);
#12018=PRODUCT_DEFINITION('Crank','Crank',#12057,#11984);
#12019=PRODUCT_DEFINITION('Handle','Handle',#12058,#11984);
#12020=PRODUCT_DEFINITION('Socket Set Screw - M5x8',
'Socket Set Screw - M5x8',#12059,#11984);
#12021=PRODUCT_DEFINITION('Cap Screw - M5x20','Cap Screw - M5x20',#12060,
#11984);
#12022=PRODUCT_DEFINITION('Pawl','Pawl',#12061,#11984);
#12023=PRODUCT_DEFINITION('Pawl (1)','Pawl (1)',#12062,#11984);
#12024=PRODUCT_DEFINITION_FORMATION('',$,#12105);
#12025=PRODUCT_DEFINITION_FORMATION('',$,#12106);
#12026=PRODUCT_DEFINITION_FORMATION('',$,#12107);
#12027=PRODUCT_DEFINITION_FORMATION('',$,#12108);
#12028=PRODUCT_DEFINITION_FORMATION('',$,#12109);
#12029=PRODUCT_DEFINITION_FORMATION('',$,#12110);
#12030=PRODUCT_DEFINITION_FORMATION('',$,#12111);
#12031=PRODUCT_DEFINITION_FORMATION('',$,#12112);
#12032=PRODUCT_DEFINITION_FORMATION('',$,#12113);
#12033=PRODUCT_DEFINITION_FORMATION('',$,#12114);
#12034=PRODUCT_DEFINITION_FORMATION('',$,#12115);
#12035=PRODUCT_DEFINITION_FORMATION('',$,#12116);
#12036=PRODUCT_DEFINITION_FORMATION('',$,#12117);
#12037=PRODUCT_DEFINITION_FORMATION('',$,#12118);
#12038=PRODUCT_DEFINITION_FORMATION('',$,#12119);
#12039=PRODUCT_DEFINITION_FORMATION('',$,#12120);
#12040=PRODUCT_DEFINITION_FORMATION('',$,#12121);
#12041=PRODUCT_DEFINITION_FORMATION('',$,#12122);
#12042=PRODUCT_DEFINITION_FORMATION('',$,#12123);
#12043=PRODUCT_DEFINITION_FORMATION('',$,#12124);
#12044=PRODUCT_DEFINITION_FORMATION('',$,#12125);
#12045=PRODUCT_DEFINITION_FORMATION('',$,#12126);
#12046=PRODUCT_DEFINITION_FORMATION('',$,#12127);
#12047=PRODUCT_DEFINITION_FORMATION('',$,#12128);
#12048=PRODUCT_DEFINITION_FORMATION('',$,#12129);
#12049=PRODUCT_DEFINITION_FORMATION('',$,#12130);
#12050=PRODUCT_DEFINITION_FORMATION('',$,#12131);
#12051=PRODUCT_DEFINITION_FORMATION('',$,#12132);
#12052=PRODUCT_DEFINITION_FORMATION('',$,#12133);
#12053=PRODUCT_DEFINITION_FORMATION('',$,#12134);
#12054=PRODUCT_DEFINITION_FORMATION('',$,#12135);
#12055=PRODUCT_DEFINITION_FORMATION('',$,#12136);
#12056=PRODUCT_DEFINITION_FORMATION('',$,#12137);
#12057=PRODUCT_DEFINITION_FORMATION('',$,#12138);
#12058=PRODUCT_DEFINITION_FORMATION('',$,#12139);
#12059=PRODUCT_DEFINITION_FORMATION('',$,#12140);
#12060=PRODUCT_DEFINITION_FORMATION('',$,#12141);
#12061=PRODUCT_DEFINITION_FORMATION('',$,#12142);
#12062=PRODUCT_DEFINITION_FORMATION('',$,#12143);
#12063=PRODUCT_RELATED_PRODUCT_CATEGORY('PAT-086','PAT-086',(#12105));
#12064=PRODUCT_RELATED_PRODUCT_CATEGORY('Base and bearing supports',
'Base and bearing supports',(#12106));
#12065=PRODUCT_RELATED_PRODUCT_CATEGORY('Base','Base',(#12107));
#12066=PRODUCT_RELATED_PRODUCT_CATEGORY('Foot','Foot',(#12108));
#12067=PRODUCT_RELATED_PRODUCT_CATEGORY('Foot (1)','Foot (1)',(#12109));
#12068=PRODUCT_RELATED_PRODUCT_CATEGORY('Bearing riser','Bearing riser',
(#12110));
#12069=PRODUCT_RELATED_PRODUCT_CATEGORY('Mounting bush','Mounting bush',
(#12111));
#12070=PRODUCT_RELATED_PRODUCT_CATEGORY('Mounting bush (1)',
'Mounting bush (1)',(#12112));
#12071=PRODUCT_RELATED_PRODUCT_CATEGORY('Bearing riser (1)',
'Bearing riser (1)',(#12113));
#12072=PRODUCT_RELATED_PRODUCT_CATEGORY('Mounting bush (2)',
'Mounting bush (2)',(#12114));
#12073=PRODUCT_RELATED_PRODUCT_CATEGORY('Mounting bush (3)',
'Mounting bush (3)',(#12115));
#12074=PRODUCT_RELATED_PRODUCT_CATEGORY('Pawl pedestal','Pawl pedestal',
(#12116));
#12075=PRODUCT_RELATED_PRODUCT_CATEGORY('Pawl pivot pin',
'Pawl pivot pin',(#12117));
#12076=PRODUCT_RELATED_PRODUCT_CATEGORY('Pawl pivot sleeve',
'Pawl pivot sleeve',(#12118));
#12077=PRODUCT_RELATED_PRODUCT_CATEGORY('Pawl pin keeper',
'Pawl pin keeper',(#12119));
#12078=PRODUCT_RELATED_PRODUCT_CATEGORY('Pawl leaf spring',
'Pawl leaf spring',(#12120));
#12079=PRODUCT_RELATED_PRODUCT_CATEGORY('Spring anchor','Spring anchor',
(#12121));
#12080=PRODUCT_RELATED_PRODUCT_CATEGORY(
'Pillow Block Bearing - 20 mm Bore','Pillow Block Bearing - 20 mm Bore',
(#12122));
#12081=PRODUCT_RELATED_PRODUCT_CATEGORY('Housing','Housing',(#12123));
#12082=PRODUCT_RELATED_PRODUCT_CATEGORY('Insert bearing',
'Insert bearing',(#12124));
#12083=PRODUCT_RELATED_PRODUCT_CATEGORY('Flat Washer - M8',
'Flat Washer - M8',(#12125));
#12084=PRODUCT_RELATED_PRODUCT_CATEGORY('M8x25 Bolt','M8x25 Bolt',(#12126));
#12085=PRODUCT_RELATED_PRODUCT_CATEGORY('M4x10 Cap Screw',
'M4x10 Cap Screw',(#12127));
#12086=PRODUCT_RELATED_PRODUCT_CATEGORY('Drum shaft and crank',
'Drum shaft and crank',(#12128));
#12087=PRODUCT_RELATED_PRODUCT_CATEGORY('Drum shaft','Drum shaft',(#12129));
#12088=PRODUCT_RELATED_PRODUCT_CATEGORY('Shaft collar','Shaft collar',(#12130));
#12089=PRODUCT_RELATED_PRODUCT_CATEGORY('Shaft collar (1)',
'Shaft collar (1)',(#12131));
#12090=PRODUCT_RELATED_PRODUCT_CATEGORY('Winding drum','Winding drum',(#12132));
#12091=PRODUCT_RELATED_PRODUCT_CATEGORY('Drum flange','Drum flange',(#12133));
#12092=PRODUCT_RELATED_PRODUCT_CATEGORY('Drum hub','Drum hub',(#12134));
#12093=PRODUCT_RELATED_PRODUCT_CATEGORY('Drum flange (1)',
'Drum flange (1)',(#12135));
#12094=PRODUCT_RELATED_PRODUCT_CATEGORY('Drum hub (1)','Drum hub (1)',(#12136));
#12095=PRODUCT_RELATED_PRODUCT_CATEGORY('Ratchet wheel','Ratchet wheel',
(#12137));
#12096=PRODUCT_RELATED_PRODUCT_CATEGORY('Crank','Crank',(#12138));
#12097=PRODUCT_RELATED_PRODUCT_CATEGORY('Handle','Handle',(#12139));
#12098=PRODUCT_RELATED_PRODUCT_CATEGORY('Socket Set Screw - M5x8',
'Socket Set Screw - M5x8',(#12140));
#12099=PRODUCT_RELATED_PRODUCT_CATEGORY('Cap Screw - M5x20',
'Cap Screw - M5x20',(#12141));
#12100=PRODUCT_RELATED_PRODUCT_CATEGORY('Pawl','Pawl',(#12142));
#12101=PRODUCT_RELATED_PRODUCT_CATEGORY('Pawl (1)','Pawl (1)',(#12143));
#12102=APPLICATION_PROTOCOL_DEFINITION('international standard',
'automotive_design',2009,#12103);
#12103=APPLICATION_CONTEXT(
'Core Data for Automotive Mechanical Design Process');
#12104=PRODUCT_CONTEXT('part definition',#12103,'mechanical');
#12105=PRODUCT('PAT-086','PAT-086',
'PAT-086',(#12104));
#12106=PRODUCT('Base and bearing supports','Base and bearing supports',
'Base and bearing supports',(#12104));
#12107=PRODUCT('Base','Base','Base',(#12104));
#12108=PRODUCT('Foot','Foot','Foot',(#12104));
#12109=PRODUCT('Foot (1)','Foot (1)','Foot (1)',(#12104));
#12110=PRODUCT('Bearing riser','Bearing riser','Bearing riser',(#12104));
#12111=PRODUCT('Mounting bush','Mounting bush','Mounting bush',(#12104));
#12112=PRODUCT('Mounting bush (1)','Mounting bush (1)','Mounting bush (1)',(#12104));
#12113=PRODUCT('Bearing riser (1)','Bearing riser (1)','Bearing riser (1)',(#12104));
#12114=PRODUCT('Mounting bush (2)','Mounting bush (2)','Mounting bush (2)',(#12104));
#12115=PRODUCT('Mounting bush (3)','Mounting bush (3)','Mounting bush (3)',(#12104));
#12116=PRODUCT('Pawl pedestal','Pawl pedestal','Pawl pedestal',(#12104));
#12117=PRODUCT('Pawl pivot pin','Pawl pivot pin','Pawl pivot pin',(#12104));
#12118=PRODUCT('Pawl pivot sleeve','Pawl pivot sleeve',
'Pawl pivot sleeve',(#12104));
#12119=PRODUCT('Pawl pin keeper','Pawl pin keeper','Pawl pin keeper',(#12104));
#12120=PRODUCT('Pawl leaf spring','Pawl leaf spring','Pawl leaf spring',
(#12104));
#12121=PRODUCT('Spring anchor','Spring anchor','Spring anchor',(#12104));
#12122=PRODUCT('Pillow Block Bearing - 20 mm Bore',
'Pillow Block Bearing - 20 mm Bore','Pillow Block Bearing - 20 mm Bore',
(#12104));
#12123=PRODUCT('Housing','Housing','Housing',(#12104));
#12124=PRODUCT('Insert bearing','Insert bearing','Insert bearing',(#12104));
#12125=PRODUCT('Flat Washer - M8','Flat Washer - M8','Flat Washer - M8',
(#12104));
#12126=PRODUCT('M8x25 Bolt','M8x25 Bolt','M8x25 Bolt',(#12104));
#12127=PRODUCT('M4x10 Cap Screw','M4x10 Cap Screw','M4x10 Cap Screw',(#12104));
#12128=PRODUCT('Drum shaft and crank','Drum shaft and crank',
'Drum shaft and crank',(#12104));
#12129=PRODUCT('Drum shaft','Drum shaft','Drum shaft',(#12104));
#12130=PRODUCT('Shaft collar','Shaft collar','Shaft collar',(#12104));
#12131=PRODUCT('Shaft collar (1)','Shaft collar (1)','Shaft collar (1)',(#12104));
#12132=PRODUCT('Winding drum','Winding drum','Winding drum',(#12104));
#12133=PRODUCT('Drum flange','Drum flange','Drum flange',(#12104));
#12134=PRODUCT('Drum hub','Drum hub','Drum hub',(#12104));
#12135=PRODUCT('Drum flange (1)','Drum flange (1)','Drum flange (1)',(#12104));
#12136=PRODUCT('Drum hub (1)','Drum hub (1)','Drum hub (1)',(#12104));
#12137=PRODUCT('Ratchet wheel','Ratchet wheel','Ratchet wheel',(#12104));
#12138=PRODUCT('Crank','Crank','Crank',(#12104));
#12139=PRODUCT('Handle','Handle','Handle',(#12104));
#12140=PRODUCT('Socket Set Screw - M5x8','Socket Set Screw - M5x8',
'Socket Set Screw - M5x8',(#12104));
#12141=PRODUCT('Cap Screw - M5x20','Cap Screw - M5x20',
'Cap Screw - M5x20',(#12104));
#12142=PRODUCT('Pawl','Pawl','Pawl',(#12104));
#12143=PRODUCT('Pawl (1)','Pawl (1)','Pawl (1)',(#12104));
#12144=PRESENTATION_STYLE_ASSIGNMENT((#12150));
#12145=PRESENTATION_STYLE_ASSIGNMENT((#12151));
#12146=PRESENTATION_STYLE_ASSIGNMENT((#12152));
#12147=PRESENTATION_STYLE_ASSIGNMENT((#12153));
#12148=PRESENTATION_STYLE_ASSIGNMENT((#12154));
#12149=PRESENTATION_STYLE_ASSIGNMENT((#12155));
#12150=SURFACE_STYLE_USAGE(.BOTH.,#12156);
#12151=SURFACE_STYLE_USAGE(.BOTH.,#12157);
#12152=SURFACE_STYLE_USAGE(.BOTH.,#12158);
#12153=SURFACE_STYLE_USAGE(.BOTH.,#12159);
#12154=SURFACE_STYLE_USAGE(.BOTH.,#12160);
#12155=SURFACE_STYLE_USAGE(.BOTH.,#12161);
#12156=SURFACE_SIDE_STYLE('',(#12162));
#12157=SURFACE_SIDE_STYLE('',(#12163));
#12158=SURFACE_SIDE_STYLE('',(#12164));
#12159=SURFACE_SIDE_STYLE('',(#12165));
#12160=SURFACE_SIDE_STYLE('',(#12166));
#12161=SURFACE_SIDE_STYLE('',(#12167));
#12162=SURFACE_STYLE_FILL_AREA(#12168);
#12163=SURFACE_STYLE_FILL_AREA(#12169);
#12164=SURFACE_STYLE_FILL_AREA(#12170);
#12165=SURFACE_STYLE_FILL_AREA(#12171);
#12166=SURFACE_STYLE_FILL_AREA(#12172);
#12167=SURFACE_STYLE_FILL_AREA(#12173);
#12168=FILL_AREA_STYLE('Steel - Satin',(#12174));
#12169=FILL_AREA_STYLE('CAD Library Painted - Deep blue',(#12175));
#12170=FILL_AREA_STYLE('CAD Library Painted - Steel gray',(#12176));
#12171=FILL_AREA_STYLE('CAD Library Painted - Engineering blue',(#12177));
#12172=FILL_AREA_STYLE('CAD Library Painted - Graphite',(#12178));
#12173=FILL_AREA_STYLE('CAD Library Painted - Light blue',(#12179));
#12174=FILL_AREA_STYLE_COLOUR('Steel - Satin',#12180);
#12175=FILL_AREA_STYLE_COLOUR('CAD Library Painted - Deep blue',#12181);
#12176=FILL_AREA_STYLE_COLOUR('CAD Library Painted - Steel gray',#12182);
#12177=FILL_AREA_STYLE_COLOUR('CAD Library Painted - Engineering blue',
#12183);
#12178=FILL_AREA_STYLE_COLOUR('CAD Library Painted - Graphite',#12184);
#12179=FILL_AREA_STYLE_COLOUR('CAD Library Painted - Light blue',#12185);
#12180=COLOUR_RGB('Steel - Satin',0.627450980392157,0.627450980392157,0.627450980392157);
#12181=COLOUR_RGB('CAD Library Painted - Deep blue',0.0784313725490196,
0.203921568627451,0.349019607843137);
#12182=COLOUR_RGB('CAD Library Painted - Steel gray',0.592156862745098,
0.631372549019608,0.67843137254902);
#12183=COLOUR_RGB('CAD Library Painted - Engineering blue',0.12156862745098,
0.356862745098039,0.6);
#12184=COLOUR_RGB('CAD Library Painted - Graphite',0.168627450980392,0.192156862745098,
0.231372549019608);
#12185=COLOUR_RGB('CAD Library Painted - Light blue',0.286274509803922,
0.552941176470588,0.780392156862745);
#12186=COLOUR_RGB('Dark Blue',0.08,0.2,0.34);
#12187=FILL_AREA_STYLE_COLOUR('',#12186);
#12188=FILL_AREA_STYLE('',(#12187));
#12189=SURFACE_STYLE_FILL_AREA(#12188);
#12190=SURFACE_SIDE_STYLE('',(#12189));
#12191=SURFACE_STYLE_USAGE(.BOTH.,#12190);
#12192=PRESENTATION_STYLE_ASSIGNMENT((#12191));
#12193=COLOUR_RGB('Light Blue',0.38,0.62,0.78);
#12194=FILL_AREA_STYLE_COLOUR('',#12193);
#12195=FILL_AREA_STYLE('',(#12194));
#12196=SURFACE_STYLE_FILL_AREA(#12195);
#12197=SURFACE_SIDE_STYLE('',(#12196));
#12198=SURFACE_STYLE_USAGE(.BOTH.,#12197);
#12199=PRESENTATION_STYLE_ASSIGNMENT((#12198));
#12200=COLOUR_RGB('Sky Blue',0.24,0.69,0.87);
#12201=FILL_AREA_STYLE_COLOUR('',#12200);
#12202=FILL_AREA_STYLE('',(#12201));
#12203=SURFACE_STYLE_FILL_AREA(#12202);
#12204=SURFACE_SIDE_STYLE('',(#12203));
#12205=SURFACE_STYLE_USAGE(.BOTH.,#12204);
#12206=PRESENTATION_STYLE_ASSIGNMENT((#12205));
#12207=COLOUR_RGB('Grey',0.48,0.52,0.57);
#12208=FILL_AREA_STYLE_COLOUR('',#12207);
#12209=FILL_AREA_STYLE('',(#12208));
#12210=SURFACE_STYLE_FILL_AREA(#12209);
#12211=SURFACE_SIDE_STYLE('',(#12210));
#12212=SURFACE_STYLE_USAGE(.BOTH.,#12211);
#12213=PRESENTATION_STYLE_ASSIGNMENT((#12212));
#12214=COLOUR_RGB('Black',0.12,0.14,0.17);
#12215=FILL_AREA_STYLE_COLOUR('',#12214);
#12216=FILL_AREA_STYLE('',(#12215));
#12217=SURFACE_STYLE_FILL_AREA(#12216);
#12218=SURFACE_SIDE_STYLE('',(#12217));
#12219=SURFACE_STYLE_USAGE(.BOTH.,#12218);
#12220=PRESENTATION_STYLE_ASSIGNMENT((#12219));
#12221=COLOUR_RGB('Off White',0.89,0.88,0.83);
#12222=FILL_AREA_STYLE_COLOUR('',#12221);
#12223=FILL_AREA_STYLE('',(#12222));
#12224=SURFACE_STYLE_FILL_AREA(#12223);
#12225=SURFACE_SIDE_STYLE('',(#12224));
#12226=SURFACE_STYLE_USAGE(.BOTH.,#12225);
#12227=PRESENTATION_STYLE_ASSIGNMENT((#12226));
ENDSEC;
END-ISO-10303-21;
